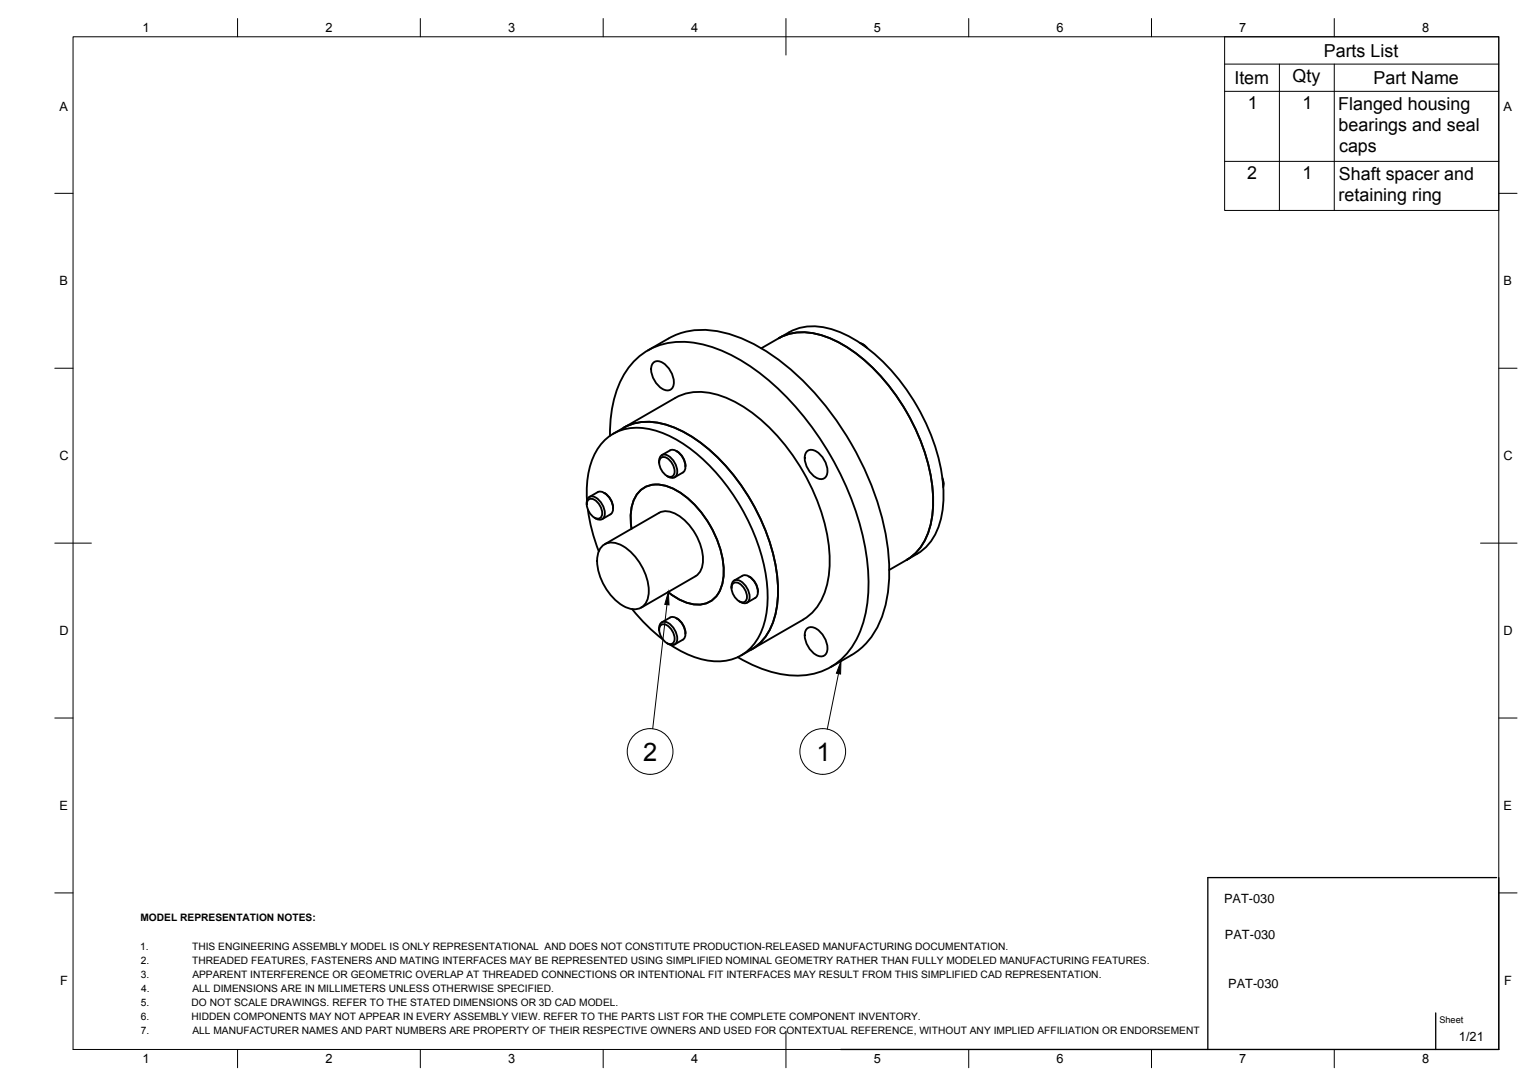
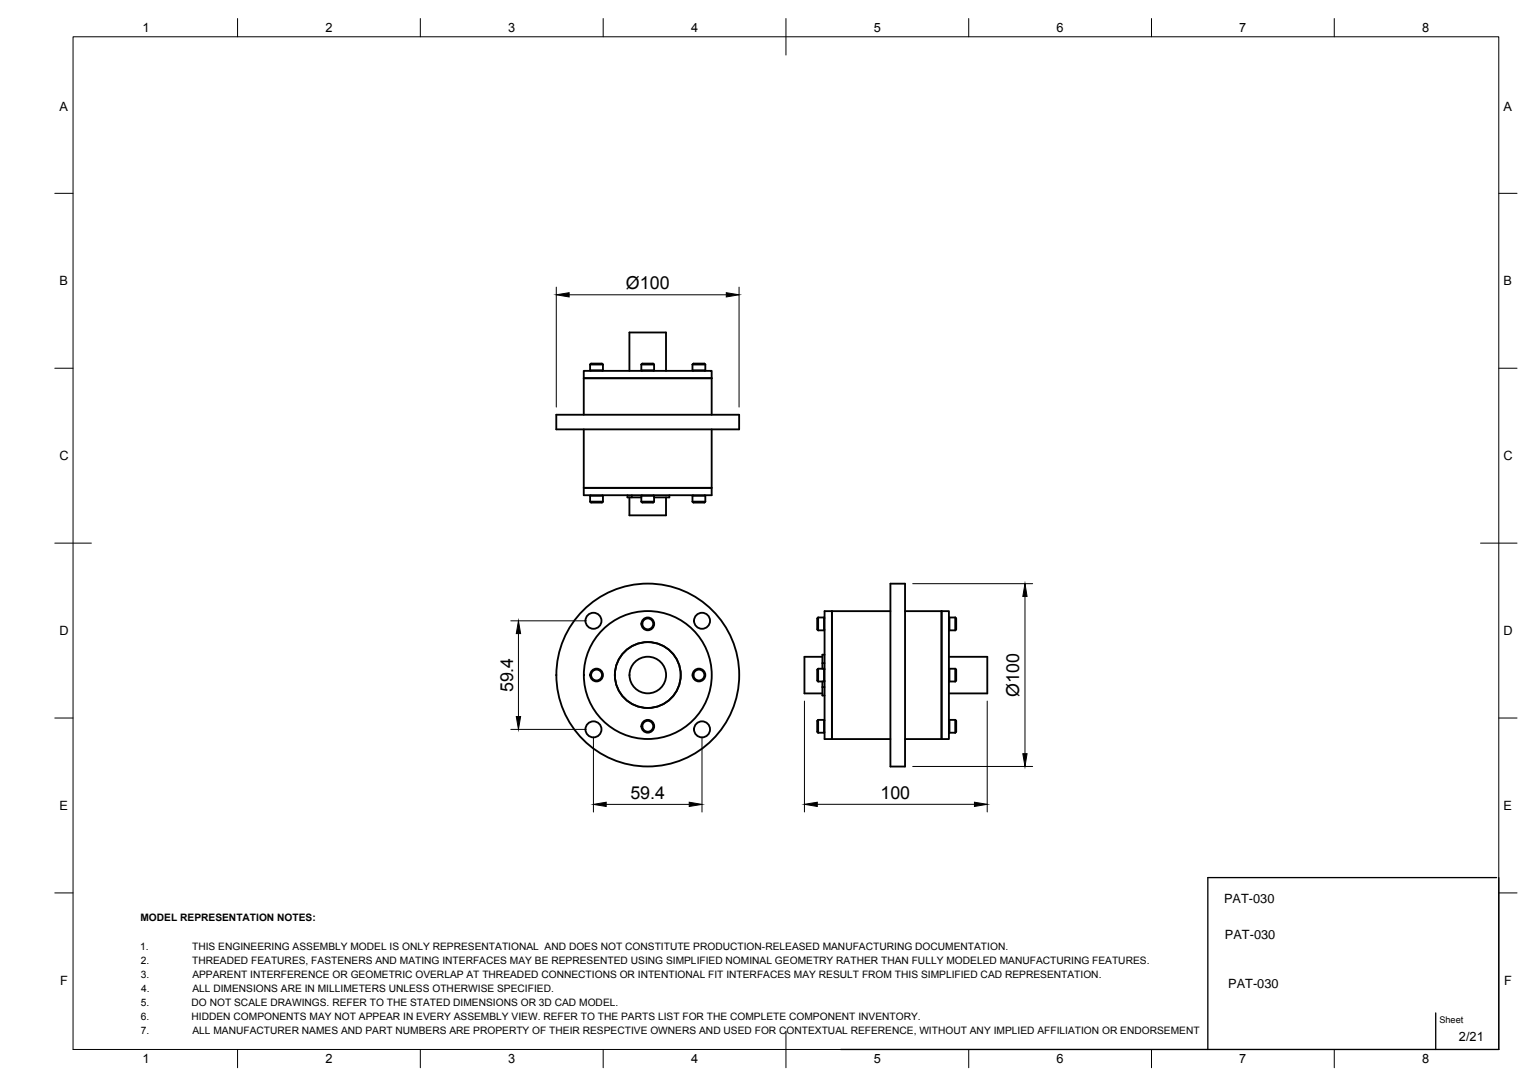
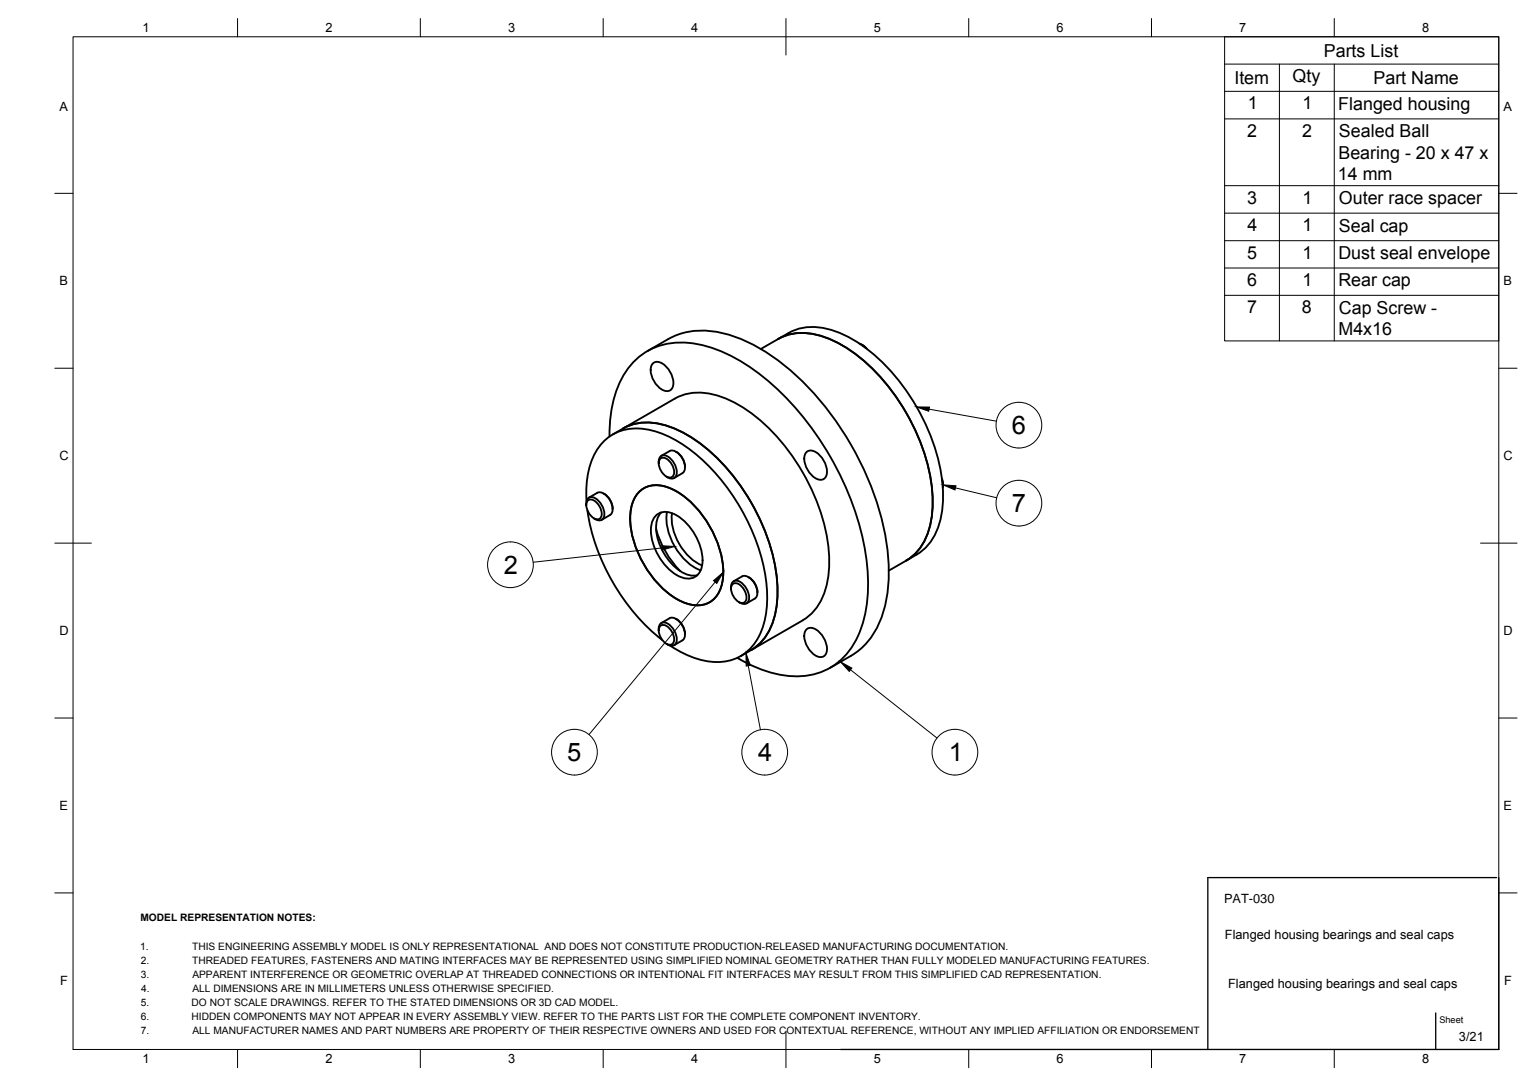
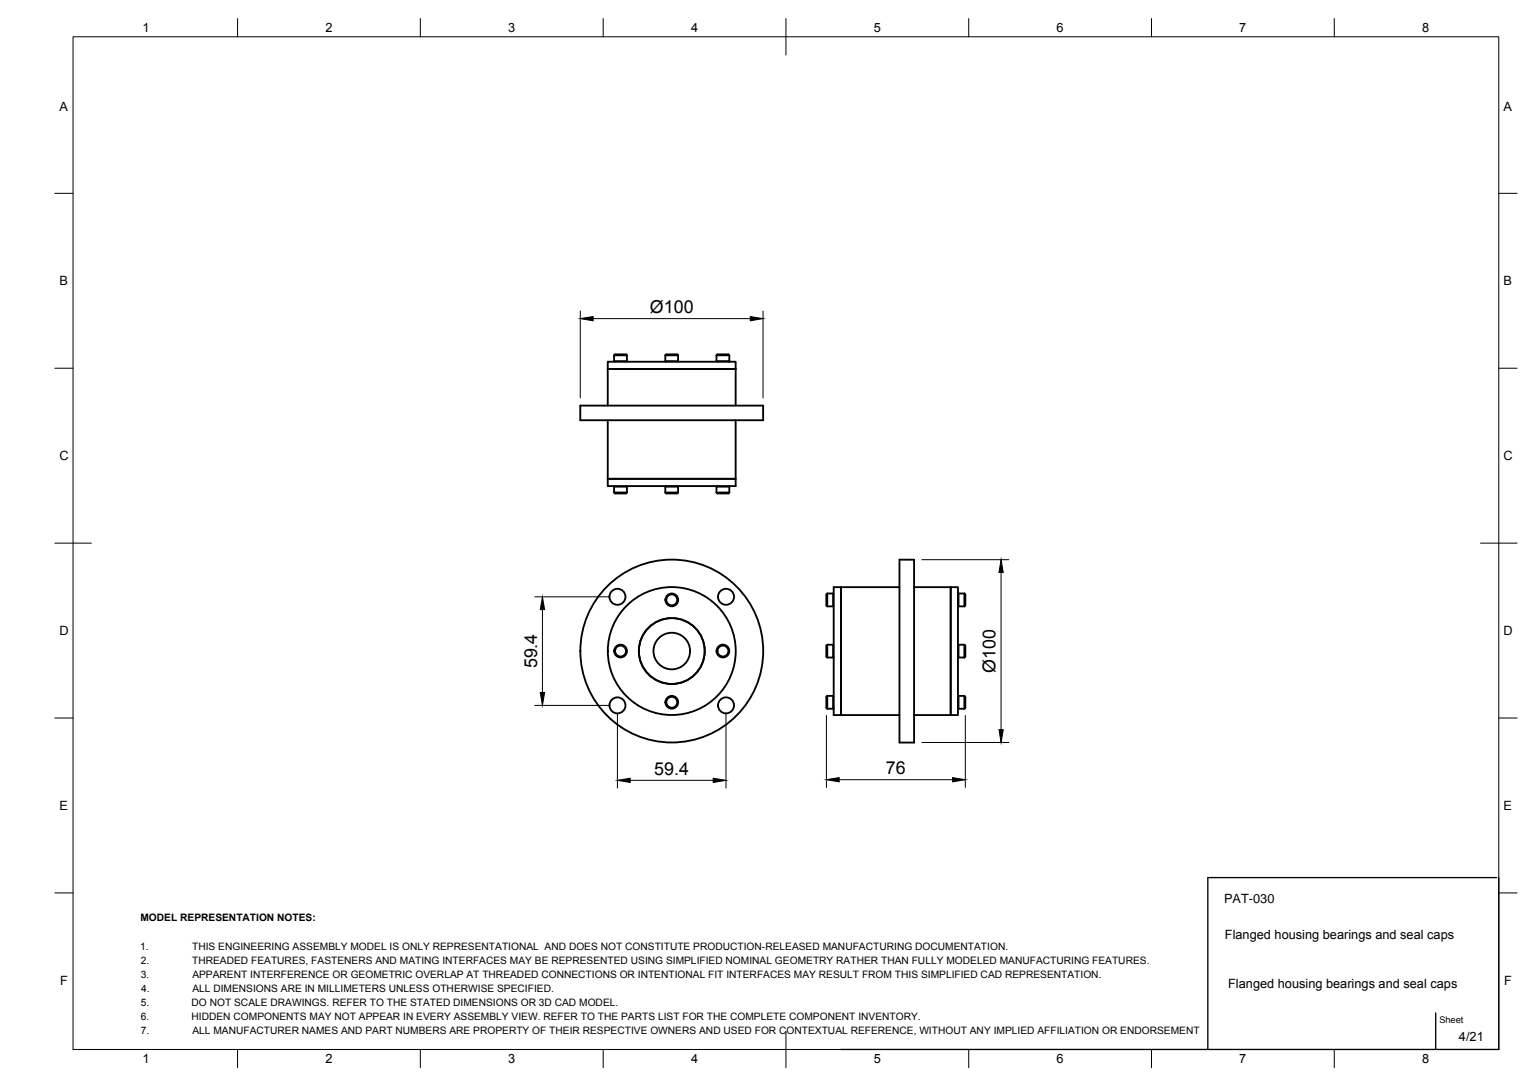
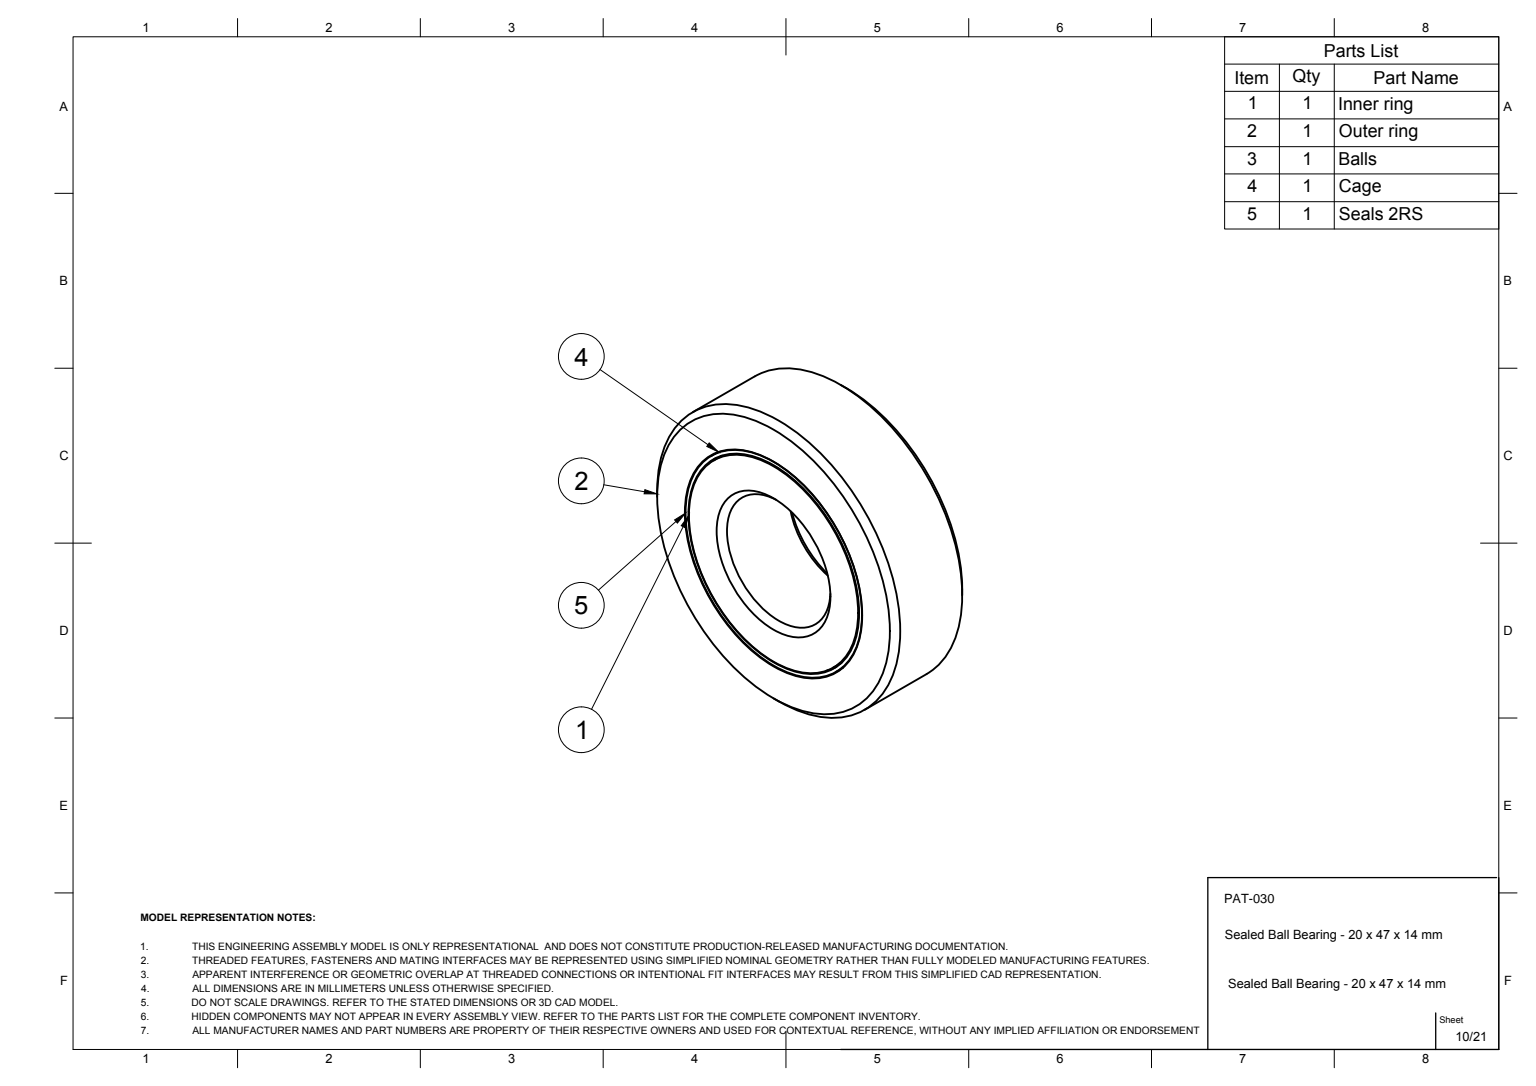
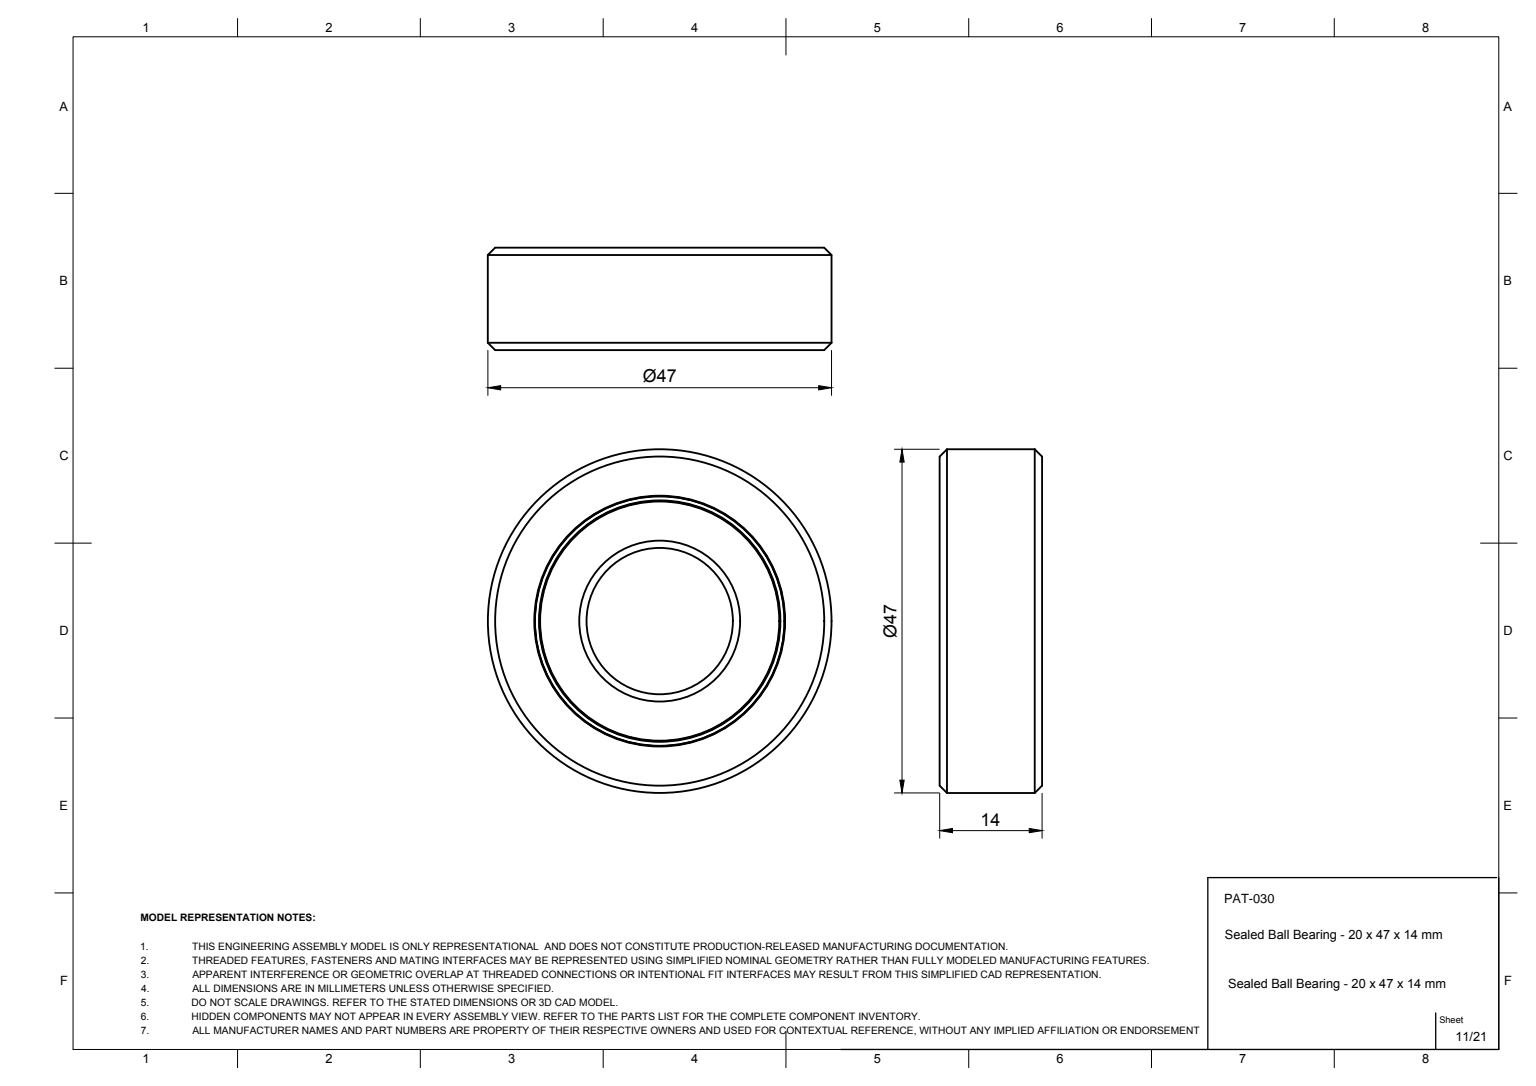
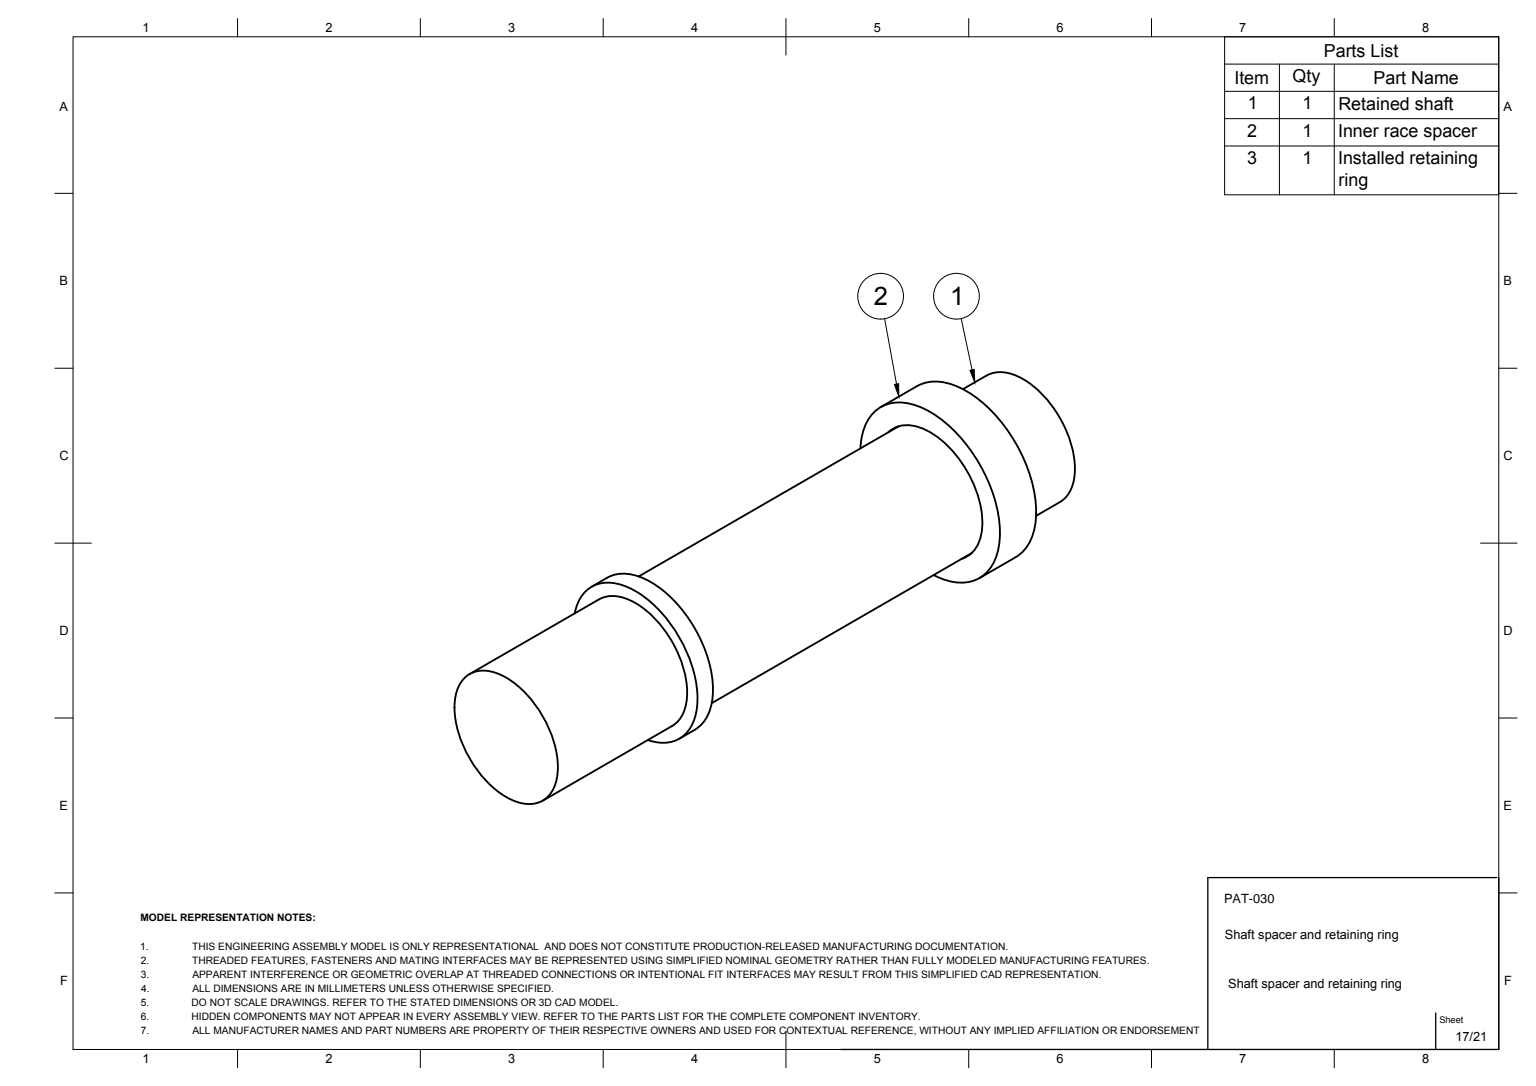
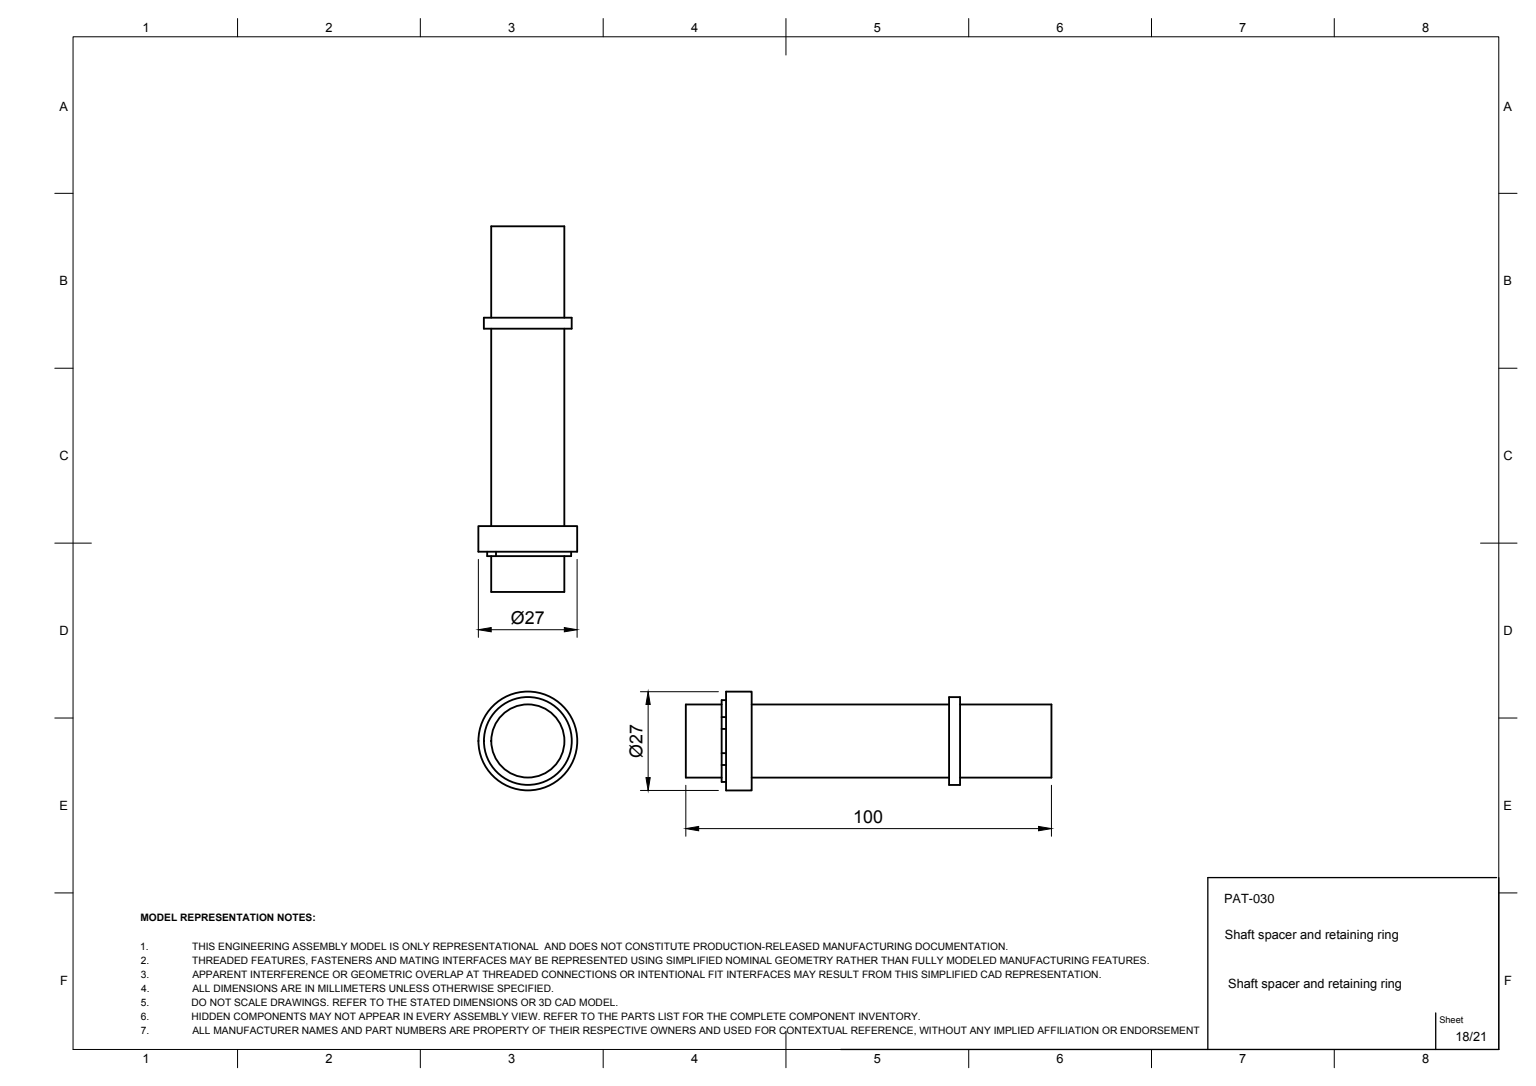
ISO-10303-21;
HEADER;
/* Generated by software containing ST-Developer
 * from STEP Tools, Inc. (www.steptools.com) 
 */

FILE_DESCRIPTION(
/* description */ ('Double-bearing flanged cartridge'),
/* implementation_level */ '2;1');

FILE_NAME(
/* name */ 'PAT-030',
/* time_stamp */ '2026-10-28T03:26:40-07:00',
/* author */ (''),
/* organization */ (''),
/* preprocessor_version */ 'ST-DEVELOPER v20.2',
/* originating_system */ 'Autodesk Translation Framework v15.17.0.0',
/* authorisation */ '');

FILE_SCHEMA (('AUTOMOTIVE_DESIGN { 1 0 10303 214 3 1 1 }'));
ENDSEC;

DATA;
#10=MECHANICAL_DESIGN_GEOMETRIC_PRESENTATION_REPRESENTATION('',(#190,#191,
#192,#193,#194,#195,#196,#197,#198,#199,#200,#201,#202,#203,#204,#205,#206,
#207,#208,#209,#210,#211),#5535);
#11=(
BOUNDED_SURFACE()
B_SPLINE_SURFACE(5,1,((#4887,#4888),(#4889,#4890),(#4891,#4892),(#4893,
#4894),(#4895,#4896),(#4897,#4898),(#4899,#4900),(#4901,#4902),(#4903,#4904),
(#4905,#4906),(#4907,#4908),(#4909,#4910),(#4911,#4912),(#4913,#4914),(#4915,
#4916),(#4917,#4918),(#4919,#4920),(#4921,#4922),(#4923,#4924),(#4925,#4926),
(#4927,#4928),(#4929,#4930),(#4931,#4932),(#4933,#4934),(#4935,#4936),(#4937,
#4938),(#4939,#4940),(#4941,#4942),(#4943,#4944),(#4945,#4946),(#4947,#4948),
(#4949,#4950),(#4951,#4952),(#4953,#4954),(#4955,#4956),(#4957,#4958),(#4959,
#4960),(#4961,#4962),(#4963,#4964),(#4965,#4966),(#4967,#4968),(#4969,#4970),
(#4971,#4972),(#4973,#4974),(#4975,#4976),(#4977,#4978),(#4979,#4980),(#4981,
#4982),(#4983,#4984),(#4985,#4986),(#4987,#4988),(#4989,#4990),(#4991,#4992),
(#4993,#4994),(#4995,#4996),(#4997,#4998),(#4999,#5000),(#5001,#5002),(#5003,
#5004),(#5005,#5006),(#5007,#5008),(#5009,#5010),(#5011,#5012),(#5013,#5014),
(#5015,#5016),(#5017,#5018),(#5019,#5020),(#5021,#5022),(#5023,#5024),(#5025,
#5026),(#5027,#5028),(#5029,#5030),(#5031,#5032),(#5033,#5034),(#5035,#5036),
(#5037,#5038),(#5039,#5040),(#5041,#5042),(#5043,#5044),(#5045,#5046),(#5047,
#5048),(#5049,#5050),(#5051,#5052),(#5053,#5054),(#5055,#5056),(#5057,#5058),
(#5059,#5060),(#5061,#5062),(#5063,#5064),(#5065,#5066),(#5067,#5068),(#5069,
#5070),(#5071,#5072),(#5073,#5074),(#5075,#5076),(#5077,#5078),(#5079,#5080),
(#5081,#5082),(#5083,#5084),(#5085,#5086),(#5087,#5088),(#5089,#5090),(#5091,
#5092),(#5093,#5094),(#5095,#5096),(#5097,#5098),(#5099,#5100),(#5101,#5102),
(#5103,#5104),(#5105,#5106),(#5107,#5108),(#5109,#5110),(#5111,#5112),(#5113,
#5114),(#5115,#5116),(#5117,#5118),(#5119,#5120),(#5121,#5122),(#5123,#5124),
(#5125,#5126),(#5127,#5128),(#5129,#5130),(#5131,#5132),(#5133,#5134),(#5135,
#5136),(#5137,#5138),(#5139,#5140),(#5141,#5142),(#5143,#5144),(#5145,#5146),
(#5147,#5148),(#5149,#5150),(#5151,#5152),(#5153,#5154),(#5155,#5156),(#5157,
#5158),(#5159,#5160),(#5161,#5162),(#5163,#5164),(#5165,#5166),(#5167,#5168),
(#5169,#5170),(#5171,#5172),(#5173,#5174),(#5175,#5176),(#5177,#5178),(#5179,
#5180),(#5181,#5182),(#5183,#5184),(#5185,#5186),(#5187,#5188),(#5189,#5190),
(#5191,#5192),(#5193,#5194),(#5195,#5196),(#5197,#5198),(#5199,#5200),(#5201,
#5202),(#5203,#5204),(#5205,#5206),(#5207,#5208),(#5209,#5210),(#5211,#5212),
(#5213,#5214),(#5215,#5216),(#5217,#5218),(#5219,#5220),(#5221,#5222),(#5223,
#5224),(#5225,#5226),(#5227,#5228),(#5229,#5230),(#5231,#5232),(#5233,#5234),
(#5235,#5236),(#5237,#5238),(#5239,#5240),(#5241,#5242),(#5243,#5244),(#5245,
#5246),(#5247,#5248),(#5249,#5250),(#5251,#5252),(#5253,#5254),(#5255,#5256),
(#5257,#5258),(#5259,#5260),(#5261,#5262),(#5263,#5264),(#5265,#5266),(#5267,
#5268),(#5269,#5270),(#5271,#5272),(#5273,#5274),(#5275,#5276),(#5277,#5278),
(#5279,#5280),(#5281,#5282),(#5283,#5284),(#5285,#5286),(#5287,#5288),(#5289,
#5290),(#5291,#5292),(#5293,#5294),(#5295,#5296)),.UNSPECIFIED.,.F.,.F.,
 .F.)
B_SPLINE_SURFACE_WITH_KNOTS((6,1,1,1,1,1,1,1,1,1,1,1,1,1,1,1,1,1,1,1,1,
1,1,1,1,1,1,1,1,1,1,1,1,1,1,1,1,1,1,1,1,1,1,1,1,1,1,1,1,1,1,1,1,1,1,1,1,
1,1,1,1,1,1,1,1,1,1,1,1,1,1,1,1,1,1,1,1,1,1,1,1,1,1,1,1,1,1,1,1,1,1,1,1,
1,1,1,1,1,1,1,1,1,1,1,1,1,1,1,1,1,1,1,1,1,1,1,1,1,1,1,1,1,1,1,1,1,1,1,1,
1,1,1,1,1,1,1,1,1,1,1,1,1,1,1,1,1,1,1,1,1,1,1,1,1,1,1,1,1,1,1,1,1,1,1,1,
1,1,1,1,1,1,1,1,1,1,1,1,1,1,1,1,1,1,1,1,1,1,1,1,1,1,1,1,1,1,1,1,1,1,1,6),
(2,2),(0.,0.005,0.01,0.015,0.02,0.025,0.03,0.035,0.04,0.045,0.05,0.055,
0.06,0.065,0.07,0.075,0.08,0.085,0.09,0.095,0.1,0.105,0.11,0.115,0.12,0.125,
0.13,0.135,0.14,0.145,0.15,0.155,0.16,0.165,0.17,0.175,0.18,0.185,0.19,
0.195,0.2,0.205,0.21,0.215,0.22,0.225,0.23,0.235,0.24,0.245,0.25,0.255,
0.26,0.265,0.27,0.275,0.28,0.285,0.29,0.295,0.3,0.305,0.31,0.315,0.32,0.325,
0.33,0.335,0.34,0.345,0.35,0.355,0.36,0.365,0.37,0.375,0.38,0.385,0.39,
0.395,0.4,0.405,0.41,0.415,0.42,0.425,0.43,0.435,0.44,0.445,0.45,0.455,
0.46,0.465,0.47,0.475,0.48,0.485,0.49,0.495,0.5,0.505,0.51,0.515,0.52,0.525,
0.53,0.535,0.54,0.545,0.55,0.555,0.56,0.565,0.57,0.575,0.58,0.585,0.59,
0.595,0.6,0.605,0.61,0.615,0.62,0.625,0.63,0.635,0.64,0.645,0.65,0.655,
0.66,0.665,0.67,0.675,0.68,0.685,0.690000000000001,0.695000000000001,0.700000000000001,
0.705000000000001,0.710000000000001,0.715000000000001,0.720000000000001,
0.725000000000001,0.730000000000001,0.735000000000001,0.740000000000001,
0.745000000000001,0.750000000000001,0.755000000000001,0.760000000000001,
0.765000000000001,0.770000000000001,0.775000000000001,0.780000000000001,
0.785000000000001,0.790000000000001,0.795000000000001,0.800000000000001,
0.805000000000001,0.810000000000001,0.815000000000001,0.820000000000001,
0.825000000000001,0.830000000000001,0.835000000000001,0.840000000000001,
0.845000000000001,0.850000000000001,0.855000000000001,0.860000000000001,
0.865000000000001,0.870000000000001,0.875000000000001,0.880000000000001,
0.885000000000001,0.890000000000001,0.895000000000001,0.900000000000001,
0.905000000000001,0.910000000000001,0.915000000000001,0.920000000000001,
0.925000000000001,0.930000000000001,0.935000000000001,0.940000000000001,
0.945000000000001,0.950000000000001,0.955000000000001,0.960000000000001,
0.965000000000001,0.970000000000001,0.975000000000001,0.980000000000001,
0.985000000000001,0.990000000000001,0.995000000000001,1.),(0.,0.12),
 .UNSPECIFIED.)
GEOMETRIC_REPRESENTATION_ITEM()
RATIONAL_B_SPLINE_SURFACE(((1.,1.),(1.,1.),(1.,1.),(1.,1.),(1.,1.),(1.,
1.),(1.,1.),(1.,1.),(1.,1.),(1.,1.),(1.,1.),(1.,1.),(1.,1.),(1.,1.),(1.,
1.),(1.,1.),(1.,1.),(1.,1.),(1.,1.),(1.,1.),(1.,1.),(1.,1.),(1.,1.),(1.,
1.),(1.,1.),(1.,1.),(1.,1.),(1.,1.),(1.,1.),(1.,1.),(1.,1.),(1.,1.),(1.,
1.),(1.,1.),(1.,1.),(1.,1.),(1.,1.),(1.,1.),(1.,1.),(1.,1.),(1.,1.),(1.,
1.),(1.,1.),(1.,1.),(1.,1.),(1.,1.),(1.,1.),(1.,1.),(1.,1.),(1.,1.),(1.,
1.),(1.,1.),(1.,1.),(1.,1.),(1.,1.),(1.,1.),(1.,1.),(1.,1.),(1.,1.),(1.,
1.),(1.,1.),(1.,1.),(1.,1.),(1.,1.),(1.,1.),(1.,1.),(1.,1.),(1.,1.),(1.,
1.),(1.,1.),(1.,1.),(1.,1.),(1.,1.),(1.,1.),(1.,1.),(1.,1.),(1.,1.),(1.,
1.),(1.,1.),(1.,1.),(1.,1.),(1.,1.),(1.,1.),(1.,1.),(1.,1.),(1.,1.),(1.,
1.),(1.,1.),(1.,1.),(1.,1.),(1.,1.),(1.,1.),(1.,1.),(1.,1.),(1.,1.),(1.,
1.),(1.,1.),(1.,1.),(1.,1.),(1.,1.),(1.,1.),(1.,1.),(1.,1.),(1.,1.),(1.,
1.),(1.,1.),(1.,1.),(1.,1.),(1.,1.),(1.,1.),(1.,1.),(1.,1.),(1.,1.),(1.,
1.),(1.,1.),(1.,1.),(1.,1.),(1.,1.),(1.,1.),(1.,1.),(1.,1.),(1.,1.),(1.,
1.),(1.,1.),(1.,1.),(1.,1.),(1.,1.),(1.,1.),(1.,1.),(1.,1.),(1.,1.),(1.,
1.),(1.,1.),(1.,1.),(1.,1.),(1.,1.),(1.,1.),(1.,1.),(1.,1.),(1.,1.),(1.,
1.),(1.,1.),(1.,1.),(1.,1.),(1.,1.),(1.,1.),(1.,1.),(1.,1.),(1.,1.),(1.,
1.),(1.,1.),(1.,1.),(1.,1.),(1.,1.),(1.,1.),(1.,1.),(1.,1.),(1.,1.),(1.,
1.),(1.,1.),(1.,1.),(1.,1.),(1.,1.),(1.,1.),(1.,1.),(1.,1.),(1.,1.),(1.,
1.),(1.,1.),(1.,1.),(1.,1.),(1.,1.),(1.,1.),(1.,1.),(1.,1.),(1.,1.),(1.,
1.),(1.,1.),(1.,1.),(1.,1.),(1.,1.),(1.,1.),(1.,1.),(1.,1.),(1.,1.),(1.,
1.),(1.,1.),(1.,1.),(1.,1.),(1.,1.),(1.,1.),(1.,1.),(1.,1.),(1.,1.),(1.,
1.),(1.,1.),(1.,1.),(1.,1.),(1.,1.),(1.,1.),(1.,1.),(1.,1.),(1.,1.),(1.,
1.),(1.,1.)))
REPRESENTATION_ITEM('')
SURFACE()
);
#12=(
BOUNDED_CURVE()
B_SPLINE_CURVE(5,(#4671,#4672,#4673,#4674,#4675,#4676,#4677,#4678,#4679,
#4680,#4681,#4682,#4683,#4684,#4685,#4686,#4687,#4688,#4689,#4690,#4691,
#4692,#4693,#4694,#4695,#4696,#4697,#4698,#4699,#4700,#4701,#4702,#4703,
#4704,#4705,#4706,#4707,#4708,#4709,#4710,#4711,#4712,#4713,#4714,#4715,
#4716,#4717,#4718,#4719,#4720,#4721,#4722,#4723,#4724,#4725,#4726,#4727,
#4728,#4729,#4730,#4731,#4732,#4733,#4734,#4735,#4736,#4737,#4738,#4739,
#4740,#4741,#4742,#4743,#4744,#4745,#4746,#4747,#4748,#4749,#4750,#4751,
#4752,#4753,#4754,#4755,#4756,#4757,#4758,#4759,#4760,#4761,#4762,#4763,
#4764,#4765,#4766,#4767,#4768,#4769,#4770,#4771,#4772,#4773,#4774,#4775,
#4776,#4777,#4778,#4779,#4780,#4781,#4782,#4783,#4784,#4785,#4786,#4787,
#4788,#4789,#4790,#4791,#4792,#4793,#4794,#4795,#4796,#4797,#4798,#4799,
#4800,#4801,#4802,#4803,#4804,#4805,#4806,#4807,#4808,#4809,#4810,#4811,
#4812,#4813,#4814,#4815,#4816,#4817,#4818,#4819,#4820,#4821,#4822,#4823,
#4824,#4825,#4826,#4827,#4828,#4829,#4830,#4831,#4832,#4833,#4834,#4835,
#4836,#4837,#4838,#4839,#4840,#4841,#4842,#4843,#4844,#4845,#4846,#4847,
#4848,#4849,#4850,#4851,#4852,#4853,#4854,#4855,#4856,#4857,#4858,#4859,
#4860,#4861,#4862,#4863,#4864,#4865),.UNSPECIFIED.,.F.,.F.)
B_SPLINE_CURVE_WITH_KNOTS((6,1,1,1,1,1,1,1,1,1,1,1,1,1,1,1,1,1,1,1,1,1,
1,1,1,1,1,1,1,1,1,1,1,1,1,1,1,1,1,1,1,1,1,1,1,1,1,1,1,1,1,1,1,1,1,1,1,1,
1,1,1,1,1,1,1,1,1,1,1,1,1,1,1,1,1,1,1,1,1,1,1,1,1,1,1,1,1,1,1,1,1,1,1,1,
1,1,1,1,1,1,1,1,1,1,1,1,1,1,1,1,1,1,1,1,1,1,1,1,1,1,1,1,1,1,1,1,1,1,1,1,
1,1,1,1,1,1,1,1,1,1,1,1,1,1,1,1,1,1,1,1,1,1,1,1,1,1,1,1,1,1,1,1,1,1,1,1,
1,1,1,1,1,1,1,1,1,1,1,1,1,1,1,1,1,1,1,1,1,1,1,1,6),(0.02759962388435,0.03,
0.035,0.04,0.045,0.05,0.055,0.06,0.065,0.07,0.075,0.08,0.085,0.09,0.095,
0.1,0.105,0.11,0.115,0.12,0.125,0.13,0.135,0.14,0.145,0.15,0.155,0.16,0.165,
0.17,0.175,0.18,0.185,0.19,0.195,0.2,0.205,0.21,0.215,0.22,0.225,0.23,0.235,
0.24,0.245,0.25,0.255,0.26,0.265,0.27,0.275,0.28,0.285,0.29,0.295,0.3,0.305,
0.31,0.315,0.32,0.325,0.33,0.335,0.34,0.345,0.35,0.355,0.36,0.365,0.37,
0.375,0.38,0.385,0.39,0.395,0.4,0.405,0.41,0.415,0.42,0.425,0.43,0.435,
0.44,0.445,0.45,0.455,0.46,0.465,0.47,0.475,0.48,0.485,0.49,0.495,0.5,0.505,
0.51,0.515,0.52,0.525,0.53,0.535,0.54,0.545,0.55,0.555,0.56,0.565,0.57,
0.575,0.58,0.585,0.59,0.595,0.6,0.605,0.61,0.615,0.62,0.625,0.63,0.635,
0.64,0.645,0.65,0.655,0.66,0.665,0.67,0.675,0.68,0.685,0.690000000000001,
0.695000000000001,0.700000000000001,0.705000000000001,0.710000000000001,
0.715000000000001,0.720000000000001,0.725000000000001,0.730000000000001,
0.735000000000001,0.740000000000001,0.745000000000001,0.750000000000001,
0.755000000000001,0.760000000000001,0.765000000000001,0.770000000000001,
0.775000000000001,0.780000000000001,0.785000000000001,0.790000000000001,
0.795000000000001,0.800000000000001,0.805000000000001,0.810000000000001,
0.815000000000001,0.820000000000001,0.825000000000001,0.830000000000001,
0.835000000000001,0.840000000000001,0.845000000000001,0.850000000000001,
0.855000000000001,0.860000000000001,0.865000000000001,0.870000000000001,
0.875000000000001,0.880000000000001,0.885000000000001,0.890000000000001,
0.895000000000001,0.900000000000001,0.905000000000001,0.910000000000001,
0.915000000000001,0.920000000000001,0.925000000000001,0.930000000000001,
0.935000000000001,0.940000000000001,0.945000000000001,0.950000000000001,
0.955000000000001,0.960000000000001,0.965000000000001,0.970000000000001,
0.972400376115677),.UNSPECIFIED.)
CURVE()
GEOMETRIC_REPRESENTATION_ITEM()
RATIONAL_B_SPLINE_CURVE((1.,1.,1.,1.,1.,1.,1.,1.,1.,1.,1.,1.,1.,1.,1.,1.,
1.,1.,1.,1.,1.,1.,1.,1.,1.,1.,1.,1.,1.,1.,1.,1.,1.,1.,1.,1.,1.,1.,1.,1.,
1.,1.,1.,1.,1.,1.,1.,1.,1.,1.,1.,1.,1.,1.,1.,1.,1.,1.,1.,1.,1.,1.,1.,1.,
1.,1.,1.,1.,1.,1.,1.,1.,1.,1.,1.,1.,1.,1.,1.,1.,1.,1.,1.,1.,1.,1.,1.,1.,
1.,1.,1.,1.,1.,1.,1.,1.,1.,1.,1.,1.,1.,1.,1.,1.,1.,1.,1.,1.,1.,1.,1.,1.,
1.,1.,1.,1.,1.,1.,1.,1.,1.,1.,1.,1.,1.,1.,1.,1.,1.,1.,1.,1.,1.,1.,1.,1.,
1.,1.,1.,1.,1.,1.,1.,1.,1.,1.,1.,1.,1.,1.,1.,1.,1.,1.,1.,1.,1.,1.,1.,1.,
1.,1.,1.,1.,1.,1.,1.,1.,1.,1.,1.,1.,1.,1.,1.,1.,1.,1.,1.,1.,1.,1.,1.,1.,
1.,1.,1.,1.,1.,1.,1.,1.,1.,1.,1.))
REPRESENTATION_ITEM('')
);
#13=(
BOUNDED_CURVE()
B_SPLINE_CURVE(5,(#5297,#5298,#5299,#5300,#5301,#5302,#5303,#5304,#5305,
#5306,#5307,#5308,#5309,#5310,#5311,#5312,#5313,#5314,#5315,#5316,#5317,
#5318,#5319,#5320,#5321,#5322,#5323,#5324,#5325,#5326,#5327,#5328,#5329,
#5330,#5331,#5332,#5333,#5334,#5335,#5336,#5337,#5338,#5339,#5340,#5341,
#5342,#5343,#5344,#5345,#5346,#5347,#5348,#5349,#5350,#5351,#5352,#5353,
#5354,#5355,#5356,#5357,#5358,#5359,#5360,#5361,#5362,#5363,#5364,#5365,
#5366,#5367,#5368,#5369,#5370,#5371,#5372,#5373,#5374,#5375,#5376,#5377,
#5378,#5379,#5380,#5381,#5382,#5383,#5384,#5385,#5386,#5387,#5388,#5389,
#5390,#5391,#5392,#5393,#5394,#5395,#5396,#5397,#5398,#5399,#5400,#5401,
#5402,#5403,#5404,#5405,#5406,#5407,#5408,#5409,#5410,#5411,#5412,#5413,
#5414,#5415,#5416,#5417,#5418,#5419,#5420,#5421,#5422,#5423,#5424,#5425,
#5426,#5427,#5428,#5429,#5430,#5431,#5432,#5433,#5434,#5435,#5436,#5437,
#5438,#5439,#5440,#5441,#5442,#5443,#5444,#5445,#5446,#5447,#5448,#5449,
#5450,#5451,#5452,#5453,#5454,#5455,#5456,#5457,#5458,#5459,#5460,#5461,
#5462,#5463,#5464,#5465,#5466,#5467,#5468,#5469,#5470,#5471,#5472,#5473,
#5474,#5475,#5476,#5477,#5478,#5479,#5480,#5481,#5482,#5483,#5484,#5485,
#5486,#5487,#5488,#5489,#5490,#5491),.UNSPECIFIED.,.F.,.F.)
B_SPLINE_CURVE_WITH_KNOTS((6,1,1,1,1,1,1,1,1,1,1,1,1,1,1,1,1,1,1,1,1,1,
1,1,1,1,1,1,1,1,1,1,1,1,1,1,1,1,1,1,1,1,1,1,1,1,1,1,1,1,1,1,1,1,1,1,1,1,
1,1,1,1,1,1,1,1,1,1,1,1,1,1,1,1,1,1,1,1,1,1,1,1,1,1,1,1,1,1,1,1,1,1,1,1,
1,1,1,1,1,1,1,1,1,1,1,1,1,1,1,1,1,1,1,1,1,1,1,1,1,1,1,1,1,1,1,1,1,1,1,1,
1,1,1,1,1,1,1,1,1,1,1,1,1,1,1,1,1,1,1,1,1,1,1,1,1,1,1,1,1,1,1,1,1,1,1,1,
1,1,1,1,1,1,1,1,1,1,1,1,1,1,1,1,1,1,1,1,1,1,1,1,6),(0.02759962388435,0.03,
0.035,0.04,0.045,0.05,0.055,0.06,0.065,0.07,0.075,0.08,0.085,0.09,0.095,
0.1,0.105,0.11,0.115,0.12,0.125,0.13,0.135,0.14,0.145,0.15,0.155,0.16,0.165,
0.17,0.175,0.18,0.185,0.19,0.195,0.2,0.205,0.21,0.215,0.22,0.225,0.23,0.235,
0.24,0.245,0.25,0.255,0.26,0.265,0.27,0.275,0.28,0.285,0.29,0.295,0.3,0.305,
0.31,0.315,0.32,0.325,0.33,0.335,0.34,0.345,0.35,0.355,0.36,0.365,0.37,
0.375,0.38,0.385,0.39,0.395,0.4,0.405,0.41,0.415,0.42,0.425,0.43,0.435,
0.44,0.445,0.45,0.455,0.46,0.465,0.47,0.475,0.48,0.485,0.49,0.495,0.5,0.505,
0.51,0.515,0.52,0.525,0.53,0.535,0.54,0.545,0.55,0.555,0.56,0.565,0.57,
0.575,0.58,0.585,0.59,0.595,0.6,0.605,0.61,0.615,0.62,0.625,0.63,0.635,
0.64,0.645,0.65,0.655,0.66,0.665,0.67,0.675,0.68,0.685,0.690000000000001,
0.695000000000001,0.700000000000001,0.705000000000001,0.710000000000001,
0.715000000000001,0.720000000000001,0.725000000000001,0.730000000000001,
0.735000000000001,0.740000000000001,0.745000000000001,0.750000000000001,
0.755000000000001,0.760000000000001,0.765000000000001,0.770000000000001,
0.775000000000001,0.780000000000001,0.785000000000001,0.790000000000001,
0.795000000000001,0.800000000000001,0.805000000000001,0.810000000000001,
0.815000000000001,0.820000000000001,0.825000000000001,0.830000000000001,
0.835000000000001,0.840000000000001,0.845000000000001,0.850000000000001,
0.855000000000001,0.860000000000001,0.865000000000001,0.870000000000001,
0.875000000000001,0.880000000000001,0.885000000000001,0.890000000000001,
0.895000000000001,0.900000000000001,0.905000000000001,0.910000000000001,
0.915000000000001,0.920000000000001,0.925000000000001,0.930000000000001,
0.935000000000001,0.940000000000001,0.945000000000001,0.950000000000001,
0.955000000000001,0.960000000000001,0.965000000000001,0.970000000000001,
0.972400376115677),.UNSPECIFIED.)
CURVE()
GEOMETRIC_REPRESENTATION_ITEM()
RATIONAL_B_SPLINE_CURVE((1.,1.,1.,1.,1.,1.,1.,1.,1.,1.,1.,1.,1.,1.,1.,1.,
1.,1.,1.,1.,1.,1.,1.,1.,1.,1.,1.,1.,1.,1.,1.,1.,1.,1.,1.,1.,1.,1.,1.,1.,
1.,1.,1.,1.,1.,1.,1.,1.,1.,1.,1.,1.,1.,1.,1.,1.,1.,1.,1.,1.,1.,1.,1.,1.,
1.,1.,1.,1.,1.,1.,1.,1.,1.,1.,1.,1.,1.,1.,1.,1.,1.,1.,1.,1.,1.,1.,1.,1.,
1.,1.,1.,1.,1.,1.,1.,1.,1.,1.,1.,1.,1.,1.,1.,1.,1.,1.,1.,1.,1.,1.,1.,1.,
1.,1.,1.,1.,1.,1.,1.,1.,1.,1.,1.,1.,1.,1.,1.,1.,1.,1.,1.,1.,1.,1.,1.,1.,
1.,1.,1.,1.,1.,1.,1.,1.,1.,1.,1.,1.,1.,1.,1.,1.,1.,1.,1.,1.,1.,1.,1.,1.,
1.,1.,1.,1.,1.,1.,1.,1.,1.,1.,1.,1.,1.,1.,1.,1.,1.,1.,1.,1.,1.,1.,1.,1.,
1.,1.,1.,1.,1.,1.,1.,1.,1.,1.,1.))
REPRESENTATION_ITEM('')
);
#14=ORIENTED_CLOSED_SHELL('',*,#2343,.F.);
#15=BREP_WITH_VOIDS('Body1',#2342,(#14));
#16=ITEM_DEFINED_TRANSFORMATION($,$,#2566,#2694);
#17=ITEM_DEFINED_TRANSFORMATION($,$,#2586,#2695);
#18=ITEM_DEFINED_TRANSFORMATION($,$,#2606,#2696);
#19=ITEM_DEFINED_TRANSFORMATION($,$,#2623,#2697);
#20=ITEM_DEFINED_TRANSFORMATION($,$,#2677,#2698);
#21=ITEM_DEFINED_TRANSFORMATION($,$,#2504,#2797);
#22=ITEM_DEFINED_TRANSFORMATION($,$,#2565,#2798);
#23=ITEM_DEFINED_TRANSFORMATION($,$,#2565,#2799);
#24=ITEM_DEFINED_TRANSFORMATION($,$,#2699,#2800);
#25=ITEM_DEFINED_TRANSFORMATION($,$,#2708,#2801);
#26=ITEM_DEFINED_TRANSFORMATION($,$,#2737,#2802);
#27=ITEM_DEFINED_TRANSFORMATION($,$,#2746,#2803);
#28=ITEM_DEFINED_TRANSFORMATION($,$,#2771,#2804);
#29=ITEM_DEFINED_TRANSFORMATION($,$,#2771,#2805);
#30=ITEM_DEFINED_TRANSFORMATION($,$,#2771,#2806);
#31=ITEM_DEFINED_TRANSFORMATION($,$,#2771,#2807);
#32=ITEM_DEFINED_TRANSFORMATION($,$,#2771,#2808);
#33=ITEM_DEFINED_TRANSFORMATION($,$,#2771,#2809);
#34=ITEM_DEFINED_TRANSFORMATION($,$,#2771,#2810);
#35=ITEM_DEFINED_TRANSFORMATION($,$,#2771,#2811);
#36=ITEM_DEFINED_TRANSFORMATION($,$,#2813,#2862);
#37=ITEM_DEFINED_TRANSFORMATION($,$,#2835,#2863);
#38=ITEM_DEFINED_TRANSFORMATION($,$,#2844,#2864);
#39=ITEM_DEFINED_TRANSFORMATION($,$,#2503,#2865);
#40=ITEM_DEFINED_TRANSFORMATION($,$,#2812,#2866);
#41=(
REPRESENTATION_RELATIONSHIP($,$,#5605,#5604)
REPRESENTATION_RELATIONSHIP_WITH_TRANSFORMATION(#16)
SHAPE_REPRESENTATION_RELATIONSHIP()
);
#42=(
REPRESENTATION_RELATIONSHIP($,$,#5606,#5604)
REPRESENTATION_RELATIONSHIP_WITH_TRANSFORMATION(#17)
SHAPE_REPRESENTATION_RELATIONSHIP()
);
#43=(
REPRESENTATION_RELATIONSHIP($,$,#5607,#5604)
REPRESENTATION_RELATIONSHIP_WITH_TRANSFORMATION(#18)
SHAPE_REPRESENTATION_RELATIONSHIP()
);
#44=(
REPRESENTATION_RELATIONSHIP($,$,#5608,#5604)
REPRESENTATION_RELATIONSHIP_WITH_TRANSFORMATION(#19)
SHAPE_REPRESENTATION_RELATIONSHIP()
);
#45=(
REPRESENTATION_RELATIONSHIP($,$,#5609,#5604)
REPRESENTATION_RELATIONSHIP_WITH_TRANSFORMATION(#20)
SHAPE_REPRESENTATION_RELATIONSHIP()
);
#46=(
REPRESENTATION_RELATIONSHIP($,$,#5603,#5602)
REPRESENTATION_RELATIONSHIP_WITH_TRANSFORMATION(#21)
SHAPE_REPRESENTATION_RELATIONSHIP()
);
#47=(
REPRESENTATION_RELATIONSHIP($,$,#5604,#5602)
REPRESENTATION_RELATIONSHIP_WITH_TRANSFORMATION(#22)
SHAPE_REPRESENTATION_RELATIONSHIP()
);
#48=(
REPRESENTATION_RELATIONSHIP($,$,#5604,#5602)
REPRESENTATION_RELATIONSHIP_WITH_TRANSFORMATION(#23)
SHAPE_REPRESENTATION_RELATIONSHIP()
);
#49=(
REPRESENTATION_RELATIONSHIP($,$,#5610,#5602)
REPRESENTATION_RELATIONSHIP_WITH_TRANSFORMATION(#24)
SHAPE_REPRESENTATION_RELATIONSHIP()
);
#50=(
REPRESENTATION_RELATIONSHIP($,$,#5611,#5602)
REPRESENTATION_RELATIONSHIP_WITH_TRANSFORMATION(#25)
SHAPE_REPRESENTATION_RELATIONSHIP()
);
#51=(
REPRESENTATION_RELATIONSHIP($,$,#5612,#5602)
REPRESENTATION_RELATIONSHIP_WITH_TRANSFORMATION(#26)
SHAPE_REPRESENTATION_RELATIONSHIP()
);
#52=(
REPRESENTATION_RELATIONSHIP($,$,#5613,#5602)
REPRESENTATION_RELATIONSHIP_WITH_TRANSFORMATION(#27)
SHAPE_REPRESENTATION_RELATIONSHIP()
);
#53=(
REPRESENTATION_RELATIONSHIP($,$,#5614,#5602)
REPRESENTATION_RELATIONSHIP_WITH_TRANSFORMATION(#28)
SHAPE_REPRESENTATION_RELATIONSHIP()
);
#54=(
REPRESENTATION_RELATIONSHIP($,$,#5614,#5602)
REPRESENTATION_RELATIONSHIP_WITH_TRANSFORMATION(#29)
SHAPE_REPRESENTATION_RELATIONSHIP()
);
#55=(
REPRESENTATION_RELATIONSHIP($,$,#5614,#5602)
REPRESENTATION_RELATIONSHIP_WITH_TRANSFORMATION(#30)
SHAPE_REPRESENTATION_RELATIONSHIP()
);
#56=(
REPRESENTATION_RELATIONSHIP($,$,#5614,#5602)
REPRESENTATION_RELATIONSHIP_WITH_TRANSFORMATION(#31)
SHAPE_REPRESENTATION_RELATIONSHIP()
);
#57=(
REPRESENTATION_RELATIONSHIP($,$,#5614,#5602)
REPRESENTATION_RELATIONSHIP_WITH_TRANSFORMATION(#32)
SHAPE_REPRESENTATION_RELATIONSHIP()
);
#58=(
REPRESENTATION_RELATIONSHIP($,$,#5614,#5602)
REPRESENTATION_RELATIONSHIP_WITH_TRANSFORMATION(#33)
SHAPE_REPRESENTATION_RELATIONSHIP()
);
#59=(
REPRESENTATION_RELATIONSHIP($,$,#5614,#5602)
REPRESENTATION_RELATIONSHIP_WITH_TRANSFORMATION(#34)
SHAPE_REPRESENTATION_RELATIONSHIP()
);
#60=(
REPRESENTATION_RELATIONSHIP($,$,#5614,#5602)
REPRESENTATION_RELATIONSHIP_WITH_TRANSFORMATION(#35)
SHAPE_REPRESENTATION_RELATIONSHIP()
);
#61=(
REPRESENTATION_RELATIONSHIP($,$,#5616,#5615)
REPRESENTATION_RELATIONSHIP_WITH_TRANSFORMATION(#36)
SHAPE_REPRESENTATION_RELATIONSHIP()
);
#62=(
REPRESENTATION_RELATIONSHIP($,$,#5617,#5615)
REPRESENTATION_RELATIONSHIP_WITH_TRANSFORMATION(#37)
SHAPE_REPRESENTATION_RELATIONSHIP()
);
#63=(
REPRESENTATION_RELATIONSHIP($,$,#5618,#5615)
REPRESENTATION_RELATIONSHIP_WITH_TRANSFORMATION(#38)
SHAPE_REPRESENTATION_RELATIONSHIP()
);
#64=(
REPRESENTATION_RELATIONSHIP($,$,#5602,#5601)
REPRESENTATION_RELATIONSHIP_WITH_TRANSFORMATION(#39)
SHAPE_REPRESENTATION_RELATIONSHIP()
);
#65=(
REPRESENTATION_RELATIONSHIP($,$,#5615,#5601)
REPRESENTATION_RELATIONSHIP_WITH_TRANSFORMATION(#40)
SHAPE_REPRESENTATION_RELATIONSHIP()
);
#66=CONTEXT_DEPENDENT_SHAPE_REPRESENTATION(#41,#5567);
#67=CONTEXT_DEPENDENT_SHAPE_REPRESENTATION(#42,#5568);
#68=CONTEXT_DEPENDENT_SHAPE_REPRESENTATION(#43,#5569);
#69=CONTEXT_DEPENDENT_SHAPE_REPRESENTATION(#44,#5570);
#70=CONTEXT_DEPENDENT_SHAPE_REPRESENTATION(#45,#5571);
#71=CONTEXT_DEPENDENT_SHAPE_REPRESENTATION(#46,#5577);
#72=CONTEXT_DEPENDENT_SHAPE_REPRESENTATION(#47,#5578);
#73=CONTEXT_DEPENDENT_SHAPE_REPRESENTATION(#48,#5579);
#74=CONTEXT_DEPENDENT_SHAPE_REPRESENTATION(#49,#5580);
#75=CONTEXT_DEPENDENT_SHAPE_REPRESENTATION(#50,#5581);
#76=CONTEXT_DEPENDENT_SHAPE_REPRESENTATION(#51,#5582);
#77=CONTEXT_DEPENDENT_SHAPE_REPRESENTATION(#52,#5583);
#78=CONTEXT_DEPENDENT_SHAPE_REPRESENTATION(#53,#5584);
#79=CONTEXT_DEPENDENT_SHAPE_REPRESENTATION(#54,#5585);
#80=CONTEXT_DEPENDENT_SHAPE_REPRESENTATION(#55,#5586);
#81=CONTEXT_DEPENDENT_SHAPE_REPRESENTATION(#56,#5587);
#82=CONTEXT_DEPENDENT_SHAPE_REPRESENTATION(#57,#5588);
#83=CONTEXT_DEPENDENT_SHAPE_REPRESENTATION(#58,#5589);
#84=CONTEXT_DEPENDENT_SHAPE_REPRESENTATION(#59,#5590);
#85=CONTEXT_DEPENDENT_SHAPE_REPRESENTATION(#60,#5591);
#86=CONTEXT_DEPENDENT_SHAPE_REPRESENTATION(#61,#5596);
#87=CONTEXT_DEPENDENT_SHAPE_REPRESENTATION(#62,#5597);
#88=CONTEXT_DEPENDENT_SHAPE_REPRESENTATION(#63,#5598);
#89=CONTEXT_DEPENDENT_SHAPE_REPRESENTATION(#64,#5599);
#90=CONTEXT_DEPENDENT_SHAPE_REPRESENTATION(#65,#5600);
#91=NEXT_ASSEMBLY_USAGE_OCCURRENCE('Inner ring:1','Inner ring:1',
'Inner ring:1',#5623,#5624,'Inner ring:1');
#92=NEXT_ASSEMBLY_USAGE_OCCURRENCE('Outer ring:1','Outer ring:1',
'Outer ring:1',#5623,#5625,'Outer ring:1');
#93=NEXT_ASSEMBLY_USAGE_OCCURRENCE('Balls:1','Balls:1','Balls:1',#5623,
#5626,'Balls:1');
#94=NEXT_ASSEMBLY_USAGE_OCCURRENCE('Cage:1','Cage:1','Cage:1',#5623,#5627,
'Cage:1');
#95=NEXT_ASSEMBLY_USAGE_OCCURRENCE('Seals 2RS:1','Seals 2RS:1',
'Seals 2RS:1',#5623,#5628,'Seals 2RS:1');
#96=NEXT_ASSEMBLY_USAGE_OCCURRENCE('Flanged housing:1',
'Flanged housing:1','Flanged housing:1',#5621,#5622,'Flanged housing:1');
#97=NEXT_ASSEMBLY_USAGE_OCCURRENCE(
'Sealed Ball Bearing - 20 x 47 x 14 mm:2',
'Sealed Ball Bearing - 20 x 47 x 14 mm:2',
'Sealed Ball Bearing - 20 x 47 x 14 mm:2',#5621,#5623,
'Sealed Ball Bearing - 20 x 47 x 14 mm:2');
#98=NEXT_ASSEMBLY_USAGE_OCCURRENCE(
'Sealed Ball Bearing - 20 x 47 x 14 mm:3',
'Sealed Ball Bearing - 20 x 47 x 14 mm:3',
'Sealed Ball Bearing - 20 x 47 x 14 mm:3',#5621,#5623,
'Sealed Ball Bearing - 20 x 47 x 14 mm:3');
#99=NEXT_ASSEMBLY_USAGE_OCCURRENCE('Outer race spacer:2',
'Outer race spacer:2','Outer race spacer:2',#5621,#5629,
'Outer race spacer:2');
#100=NEXT_ASSEMBLY_USAGE_OCCURRENCE('Seal cap:2','Seal cap:2',
'Seal cap:2',#5621,#5630,'Seal cap:2');
#101=NEXT_ASSEMBLY_USAGE_OCCURRENCE('Dust seal envelope:2',
'Dust seal envelope:2','Dust seal envelope:2',#5621,#5631,
'Dust seal envelope:2');
#102=NEXT_ASSEMBLY_USAGE_OCCURRENCE('Rear cap:2','Rear cap:2',
'Rear cap:2',#5621,#5632,'Rear cap:2');
#103=NEXT_ASSEMBLY_USAGE_OCCURRENCE('Cap Screw - M4x16:2',
'Cap Screw - M4x16:2','Cap Screw - M4x16:2',#5621,#5633,
'Cap Screw - M4x16:2');
#104=NEXT_ASSEMBLY_USAGE_OCCURRENCE('Cap Screw - M4x16:3',
'Cap Screw - M4x16:3','Cap Screw - M4x16:3',#5621,#5633,
'Cap Screw - M4x16:3');
#105=NEXT_ASSEMBLY_USAGE_OCCURRENCE('Cap Screw - M4x16:4',
'Cap Screw - M4x16:4','Cap Screw - M4x16:4',#5621,#5633,
'Cap Screw - M4x16:4');
#106=NEXT_ASSEMBLY_USAGE_OCCURRENCE('Cap Screw - M4x16:5',
'Cap Screw - M4x16:5','Cap Screw - M4x16:5',#5621,#5633,
'Cap Screw - M4x16:5');
#107=NEXT_ASSEMBLY_USAGE_OCCURRENCE('Cap Screw - M4x16:6',
'Cap Screw - M4x16:6','Cap Screw - M4x16:6',#5621,#5633,
'Cap Screw - M4x16:6');
#108=NEXT_ASSEMBLY_USAGE_OCCURRENCE('Cap Screw - M4x16:7',
'Cap Screw - M4x16:7','Cap Screw - M4x16:7',#5621,#5633,
'Cap Screw - M4x16:7');
#109=NEXT_ASSEMBLY_USAGE_OCCURRENCE('Cap Screw - M4x16:8',
'Cap Screw - M4x16:8','Cap Screw - M4x16:8',#5621,#5633,
'Cap Screw - M4x16:8');
#110=NEXT_ASSEMBLY_USAGE_OCCURRENCE('Cap Screw - M4x16:9',
'Cap Screw - M4x16:9','Cap Screw - M4x16:9',#5621,#5633,
'Cap Screw - M4x16:9');
#111=NEXT_ASSEMBLY_USAGE_OCCURRENCE('Retained shaft:1',
'Retained shaft:1','Retained shaft:1',#5634,#5635,'Retained shaft:1');
#112=NEXT_ASSEMBLY_USAGE_OCCURRENCE('Inner race spacer:2',
'Inner race spacer:2','Inner race spacer:2',#5634,#5636,
'Inner race spacer:2');
#113=NEXT_ASSEMBLY_USAGE_OCCURRENCE('Installed retaining ring:2',
'Installed retaining ring:2','Installed retaining ring:2',#5634,#5637,
'Installed retaining ring:2');
#114=NEXT_ASSEMBLY_USAGE_OCCURRENCE(
'Flanged housing bearings and seal caps:1',
'Flanged housing bearings and seal caps:1',
'Flanged housing bearings and seal caps:1',#5620,#5621,
'Flanged housing bearings and seal caps:1');
#115=NEXT_ASSEMBLY_USAGE_OCCURRENCE('Shaft spacer and retaining ring:1',
'Shaft spacer and retaining ring:1','Shaft spacer and retaining ring:1',
#5620,#5634,'Shaft spacer and retaining ring:1');
#116=B_SPLINE_CURVE_WITH_KNOTS('',3,(#3902,#3903,#3904,#3905,#3906,#3907,
#3908,#3909,#3910,#3911,#3912,#3913,#3914,#3915,#3916,#3917,#3918,#3919,
#3920,#3921,#3922,#3923),.UNSPECIFIED.,.F.,.F.,(4,2,2,2,2,2,2,2,2,2,4),
(0.0789094028588958,0.210573405340968,0.315860108011452,0.421146810681936,
0.522142632548711,0.623138454415485,0.72413427628226,0.825130098149035,
0.930416800819519,1.03570350349,1.16736750597208),.UNSPECIFIED.);
#117=B_SPLINE_CURVE_WITH_KNOTS('',3,(#3927,#3928,#3929,#3930,#3931,#3932,
#3933,#3934,#3935,#3936,#3937,#3938,#3939,#3940,#3941,#3942,#3943,#3944,
#3945,#3946,#3947,#3948),.UNSPECIFIED.,.F.,.F.,(4,2,2,2,2,2,2,2,2,2,4),
(0.0774793363974613,0.142088896491891,0.284177792983782,0.411119756996526,
0.514392970548519,0.617666184100513,0.720939397652506,0.8242126112045,0.951154575217244,
1.09324347170913,1.15785303180356),.UNSPECIFIED.);
#118=B_SPLINE_CURVE_WITH_KNOTS('',3,(#3954,#3955,#3956,#3957,#3958,#3959,
#3960,#3961,#3962,#3963,#3964,#3965,#3966,#3967,#3968,#3969,#3970,#3971,
#3972,#3973,#3974,#3975),.UNSPECIFIED.,.F.,.F.,(4,2,2,2,2,2,2,2,2,2,4),
(0.0774793363974613,0.142088896491891,0.284177792983782,0.411119756996525,
0.514392970548519,0.617666184100513,0.720939397652506,0.8242126112045,0.951154575217243,
1.09324347170913,1.15785303180356),.UNSPECIFIED.);
#119=B_SPLINE_CURVE_WITH_KNOTS('',3,(#3979,#3980,#3981,#3982,#3983,#3984,
#3985,#3986,#3987,#3988,#3989,#3990,#3991,#3992,#3993,#3994,#3995,#3996,
#3997,#3998,#3999,#4000),.UNSPECIFIED.,.F.,.F.,(4,2,2,2,2,2,2,2,2,2,4),
(0.0774793363974614,0.142088896491891,0.284177792983781,0.411119756996525,
0.514392970548519,0.617666184100512,0.720939397652506,0.824212611204499,
0.951154575217243,1.09324347170913,1.15785303180356),.UNSPECIFIED.);
#120=B_SPLINE_CURVE_WITH_KNOTS('',3,(#4004,#4005,#4006,#4007,#4008,#4009,
#4010,#4011,#4012,#4013,#4014,#4015),.UNSPECIFIED.,.F.,.F.,(4,2,2,2,2,4),
(0.0774793363974613,0.142088896491891,0.284177792983781,0.411119756996525,
0.514392970548519,0.617666184100512),.UNSPECIFIED.);
#121=B_SPLINE_CURVE_WITH_KNOTS('',3,(#4020,#4021,#4022,#4023,#4024,#4025,
#4026,#4027,#4028,#4029,#4030,#4031),.UNSPECIFIED.,.F.,.F.,(4,2,2,2,2,4),
(0.617666184100512,0.720939397652506,0.824212611204499,0.951154575217243,
1.09324347170913,1.15785303180356),.UNSPECIFIED.);
#122=B_SPLINE_CURVE_WITH_KNOTS('',3,(#4035,#4036,#4037,#4038,#4039,#4040,
#4041,#4042,#4043,#4044,#4045,#4046,#4047,#4048,#4049,#4050,#4051,#4052,
#4053,#4054,#4055,#4056),.UNSPECIFIED.,.F.,.F.,(4,2,2,2,2,2,2,2,2,2,4),
(0.0774793363974613,0.142088896491891,0.284177792983782,0.411119756996526,
0.514392970548519,0.617666184100513,0.720939397652507,0.8242126112045,0.951154575217245,
1.09324347170914,1.15785303180356),.UNSPECIFIED.);
#123=B_SPLINE_CURVE_WITH_KNOTS('',3,(#4060,#4061,#4062,#4063,#4064,#4065,
#4066,#4067,#4068,#4069,#4070,#4071,#4072,#4073,#4074,#4075,#4076,#4077,
#4078,#4079,#4080,#4081),.UNSPECIFIED.,.F.,.F.,(4,2,2,2,2,2,2,2,2,2,4),
(0.0774793363974613,0.142088896491891,0.284177792983782,0.411119756996526,
0.514392970548519,0.617666184100513,0.720939397652506,0.824212611204499,
0.951154575217243,1.09324347170913,1.15785303180356),.UNSPECIFIED.);
#124=B_SPLINE_CURVE_WITH_KNOTS('',3,(#4085,#4086,#4087,#4088,#4089,#4090,
#4091,#4092,#4093,#4094,#4095,#4096,#4097,#4098,#4099,#4100,#4101,#4102,
#4103,#4104,#4105,#4106),.UNSPECIFIED.,.F.,.F.,(4,2,2,2,2,2,2,2,2,2,4),
(0.0774793363974613,0.142088896491891,0.284177792983782,0.411119756996526,
0.514392970548519,0.617666184100513,0.720939397652506,0.8242126112045,0.951154575217244,
1.09324347170913,1.15785303180356),.UNSPECIFIED.);
#125=B_SPLINE_CURVE_WITH_KNOTS('',3,(#4110,#4111,#4112,#4113,#4114,#4115,
#4116,#4117,#4118,#4119,#4120,#4121,#4122,#4123,#4124,#4125,#4126,#4127,
#4128,#4129,#4130,#4131),.UNSPECIFIED.,.F.,.F.,(4,2,2,2,2,2,2,2,2,2,4),
(0.0774793363974613,0.142088896491891,0.284177792983782,0.411119756996526,
0.514392970548519,0.617666184100513,0.720939397652506,0.8242126112045,0.951154575217243,
1.09324347170913,1.15785303180356),.UNSPECIFIED.);
#126=B_SPLINE_CURVE_WITH_KNOTS('',3,(#4139,#4140,#4141,#4142,#4143,#4144,
#4145,#4146,#4147,#4148,#4149,#4150,#4151,#4152,#4153,#4154,#4155,#4156,
#4157,#4158,#4159,#4160),.UNSPECIFIED.,.F.,.F.,(4,2,2,2,2,2,2,2,2,2,4),
(0.0789094028588958,0.210573405340968,0.315860108011452,0.421146810681936,
0.522142632548711,0.623138454415485,0.72413427628226,0.825130098149035,
0.930416800819519,1.03570350349,1.16736750597208),.UNSPECIFIED.);
#127=B_SPLINE_CURVE_WITH_KNOTS('',3,(#4168,#4169,#4170,#4171,#4172,#4173,
#4174,#4175,#4176,#4177,#4178,#4179,#4180,#4181,#4182,#4183,#4184,#4185,
#4186,#4187,#4188,#4189),.UNSPECIFIED.,.F.,.F.,(4,2,2,2,2,2,2,2,2,2,4),
(0.0789094028588958,0.210573405340969,0.315860108011453,0.421146810681937,
0.522142632548712,0.623138454415486,0.724134276282261,0.825130098149035,
0.930416800819519,1.03570350349,1.16736750597208),.UNSPECIFIED.);
#128=B_SPLINE_CURVE_WITH_KNOTS('',3,(#4198,#4199,#4200,#4201,#4202,#4203,
#4204,#4205,#4206,#4207,#4208,#4209),.UNSPECIFIED.,.F.,.F.,(4,2,2,2,2,4),
(0.0789094028588958,0.210573405340968,0.315860108011452,0.421146810681937,
0.522142632548711,0.623138454415486),.UNSPECIFIED.);
#129=B_SPLINE_CURVE_WITH_KNOTS('',3,(#4211,#4212,#4213,#4214,#4215,#4216,
#4217,#4218,#4219,#4220,#4221,#4222),.UNSPECIFIED.,.F.,.F.,(4,2,2,2,2,4),
(0.623138454415486,0.72413427628226,0.825130098149035,0.930416800819519,
1.03570350349,1.16736750597208),.UNSPECIFIED.);
#130=B_SPLINE_CURVE_WITH_KNOTS('',3,(#4229,#4230,#4231,#4232,#4233,#4234,
#4235,#4236,#4237,#4238,#4239,#4240,#4241,#4242,#4243,#4244,#4245,#4246,
#4247,#4248,#4249,#4250),.UNSPECIFIED.,.F.,.F.,(4,2,2,2,2,2,2,2,2,2,4),
(0.0789094028588958,0.210573405340968,0.315860108011452,0.421146810681936,
0.522142632548711,0.623138454415486,0.72413427628226,0.825130098149035,
0.930416800819519,1.03570350349,1.16736750597208),.UNSPECIFIED.);
#131=B_SPLINE_CURVE_WITH_KNOTS('',3,(#4258,#4259,#4260,#4261,#4262,#4263,
#4264,#4265,#4266,#4267,#4268,#4269,#4270,#4271,#4272,#4273,#4274,#4275,
#4276,#4277,#4278,#4279),.UNSPECIFIED.,.F.,.F.,(4,2,2,2,2,2,2,2,2,2,4),
(0.0789094028588957,0.210573405340968,0.315860108011452,0.421146810681936,
0.522142632548711,0.623138454415485,0.72413427628226,0.825130098149035,
0.930416800819519,1.03570350349,1.16736750597207),.UNSPECIFIED.);
#132=B_SPLINE_CURVE_WITH_KNOTS('',3,(#4287,#4288,#4289,#4290,#4291,#4292,
#4293,#4294,#4295,#4296,#4297,#4298,#4299,#4300,#4301,#4302,#4303,#4304,
#4305,#4306,#4307,#4308),.UNSPECIFIED.,.F.,.F.,(4,2,2,2,2,2,2,2,2,2,4),
(0.0789094028588958,0.210573405340968,0.315860108011452,0.421146810681936,
0.522142632548711,0.623138454415486,0.72413427628226,0.825130098149035,
0.930416800819519,1.03570350349,1.16736750597208),.UNSPECIFIED.);
#133=B_SPLINE_CURVE_WITH_KNOTS('',3,(#4317,#4318,#4319,#4320,#4321,#4322,
#4323,#4324,#4325,#4326,#4327,#4328,#4329,#4330,#4331,#4332,#4333,#4334,
#4335,#4336,#4337,#4338),.UNSPECIFIED.,.F.,.F.,(4,2,2,2,2,2,2,2,2,2,4),
(0.0789094028588958,0.210573405340968,0.315860108011452,0.421146810681936,
0.522142632548711,0.623138454415485,0.72413427628226,0.825130098149035,
0.930416800819519,1.03570350349,1.16736750597208),.UNSPECIFIED.);
#134=B_SPLINE_CURVE_WITH_KNOTS('',3,(#4661,#4662,#4663,#4664,#4665,#4666),
 .UNSPECIFIED.,.F.,.F.,(4,2,4),(-0.12,-0.06,0.),.UNSPECIFIED.);
#135=B_SPLINE_CURVE_WITH_KNOTS('',3,(#4881,#4882,#4883,#4884,#4885,#4886),
 .UNSPECIFIED.,.F.,.F.,(4,2,4),(-0.12,-0.06,0.),.UNSPECIFIED.);
#136=SPHERICAL_SURFACE('',#2607,0.3969);
#137=SPHERICAL_SURFACE('',#2609,0.3969);
#138=SPHERICAL_SURFACE('',#2611,0.3969);
#139=SPHERICAL_SURFACE('',#2613,0.3969);
#140=SPHERICAL_SURFACE('',#2615,0.3969);
#141=SPHERICAL_SURFACE('',#2617,0.3969);
#142=SPHERICAL_SURFACE('',#2619,0.3969);
#143=SPHERICAL_SURFACE('',#2621,0.3969);
#144=SPHERICAL_SURFACE('',#2624,0.412776);
#145=SPHERICAL_SURFACE('',#2640,0.412776);
#146=SPHERICAL_SURFACE('',#2645,0.412776);
#147=SPHERICAL_SURFACE('',#2650,0.412776);
#148=SPHERICAL_SURFACE('',#2655,0.412776);
#149=SPHERICAL_SURFACE('',#2660,0.412776);
#150=SPHERICAL_SURFACE('',#2665,0.412776);
#151=SPHERICAL_SURFACE('',#2673,0.412776);
#152=CONICAL_SURFACE('',#2578,1.05,0.785398163397449);
#153=CONICAL_SURFACE('',#2585,1.05,0.785398163397449);
#154=CONICAL_SURFACE('',#2598,2.3,0.785398163397449);
#155=CONICAL_SURFACE('',#2602,2.3,0.785398163397449);
#156=CONICAL_SURFACE('',#2774,0.325,0.785398163397448);
#157=CONICAL_SURFACE('',#2778,0.335,0.785398163397448);
#158=CONICAL_SURFACE('',#2782,0.21,0.463647609000806);
#159=CONICAL_SURFACE('',#2786,0.18,0.785398163397448);
#160=TOROIDAL_SURFACE('',#2567,1.675,0.412776);
#161=TOROIDAL_SURFACE('',#2587,1.675,0.412776);
#162=SHAPE_REPRESENTATION_RELATIONSHIP('SRR','None',#5603,#176);
#163=SHAPE_REPRESENTATION_RELATIONSHIP('SRR','None',#5605,#177);
#164=SHAPE_REPRESENTATION_RELATIONSHIP('SRR','None',#5606,#178);
#165=SHAPE_REPRESENTATION_RELATIONSHIP('SRR','None',#5607,#179);
#166=SHAPE_REPRESENTATION_RELATIONSHIP('SRR','None',#5608,#180);
#167=SHAPE_REPRESENTATION_RELATIONSHIP('SRR','None',#5609,#181);
#168=SHAPE_REPRESENTATION_RELATIONSHIP('SRR','None',#5610,#182);
#169=SHAPE_REPRESENTATION_RELATIONSHIP('SRR','None',#5611,#183);
#170=SHAPE_REPRESENTATION_RELATIONSHIP('SRR','None',#5612,#184);
#171=SHAPE_REPRESENTATION_RELATIONSHIP('SRR','None',#5613,#185);
#172=SHAPE_REPRESENTATION_RELATIONSHIP('SRR','None',#5614,#186);
#173=SHAPE_REPRESENTATION_RELATIONSHIP('SRR','None',#5616,#187);
#174=SHAPE_REPRESENTATION_RELATIONSHIP('SRR','None',#5617,#188);
#175=SHAPE_REPRESENTATION_RELATIONSHIP('SRR','None',#5618,#189);
#176=ADVANCED_BREP_SHAPE_REPRESENTATION('',(#212),#5519);
#177=ADVANCED_BREP_SHAPE_REPRESENTATION('',(#213),#5521);
#178=ADVANCED_BREP_SHAPE_REPRESENTATION('',(#214),#5522);
#179=ADVANCED_BREP_SHAPE_REPRESENTATION('',(#215,#216,#217,#218,#219,#220,
#221,#222),#5523);
#180=ADVANCED_BREP_SHAPE_REPRESENTATION('',(#223),#5524);
#181=ADVANCED_BREP_SHAPE_REPRESENTATION('',(#224,#225),#5525);
#182=ADVANCED_BREP_SHAPE_REPRESENTATION('',(#226),#5526);
#183=ADVANCED_BREP_SHAPE_REPRESENTATION('',(#227),#5527);
#184=ADVANCED_BREP_SHAPE_REPRESENTATION('',(#228),#5528);
#185=ADVANCED_BREP_SHAPE_REPRESENTATION('',(#229),#5529);
#186=ADVANCED_BREP_SHAPE_REPRESENTATION('',(#15),#5530);
#187=ADVANCED_BREP_SHAPE_REPRESENTATION('',(#230),#5532);
#188=ADVANCED_BREP_SHAPE_REPRESENTATION('',(#231),#5533);
#189=ADVANCED_BREP_SHAPE_REPRESENTATION('',(#232),#5534);
#190=STYLED_ITEM('',(#5743),#212);
#191=STYLED_ITEM('',(#5764),#213);
#192=STYLED_ITEM('',(#5764),#214);
#193=STYLED_ITEM('',(#5764),#215);
#194=STYLED_ITEM('',(#5764),#216);
#195=STYLED_ITEM('',(#5764),#217);
#196=STYLED_ITEM('',(#5764),#218);
#197=STYLED_ITEM('',(#5764),#219);
#198=STYLED_ITEM('',(#5764),#220);
#199=STYLED_ITEM('',(#5764),#221);
#200=STYLED_ITEM('',(#5764),#222);
#201=STYLED_ITEM('',(#5764),#223);
#202=STYLED_ITEM('',(#5764),#224);
#203=STYLED_ITEM('',(#5764),#225);
#204=STYLED_ITEM('',(#5764),#226);
#205=STYLED_ITEM('',(#5771),#227);
#206=STYLED_ITEM('',(#5771),#228);
#207=STYLED_ITEM('',(#5757),#229);
#208=STYLED_ITEM('',(#5771),#15);
#209=STYLED_ITEM('',(#5764),#230);
#210=STYLED_ITEM('',(#5764),#231);
#211=STYLED_ITEM('',(#5778),#232);
#212=MANIFOLD_SOLID_BREP('Body1',#2324);
#213=MANIFOLD_SOLID_BREP('Body1',#2325);
#214=MANIFOLD_SOLID_BREP('Body1',#2326);
#215=MANIFOLD_SOLID_BREP('Body1',#2327);
#216=MANIFOLD_SOLID_BREP('Body2',#2328);
#217=MANIFOLD_SOLID_BREP('Body3',#2329);
#218=MANIFOLD_SOLID_BREP('Body4',#2330);
#219=MANIFOLD_SOLID_BREP('Body5',#2331);
#220=MANIFOLD_SOLID_BREP('Body6',#2332);
#221=MANIFOLD_SOLID_BREP('Body7',#2333);
#222=MANIFOLD_SOLID_BREP('Body8',#2334);
#223=MANIFOLD_SOLID_BREP('Continuous crown cage',#2335);
#224=MANIFOLD_SOLID_BREP('Body1',#2336);
#225=MANIFOLD_SOLID_BREP('Body2',#2337);
#226=MANIFOLD_SOLID_BREP('Body1',#2338);
#227=MANIFOLD_SOLID_BREP('Body1',#2339);
#228=MANIFOLD_SOLID_BREP('Body1',#2340);
#229=MANIFOLD_SOLID_BREP('Body1',#2341);
#230=MANIFOLD_SOLID_BREP('Body1',#2344);
#231=MANIFOLD_SOLID_BREP('Body1',#2345);
#232=MANIFOLD_SOLID_BREP('Body1',#2346);
#233=FACE_BOUND('',#531,.T.);
#234=FACE_BOUND('',#532,.T.);
#235=FACE_BOUND('',#533,.T.);
#236=FACE_BOUND('',#534,.T.);
#237=FACE_BOUND('',#535,.T.);
#238=FACE_BOUND('',#537,.T.);
#239=FACE_BOUND('',#538,.T.);
#240=FACE_BOUND('',#539,.T.);
#241=FACE_BOUND('',#540,.T.);
#242=FACE_BOUND('',#541,.T.);
#243=FACE_BOUND('',#547,.T.);
#244=FACE_BOUND('',#548,.T.);
#245=FACE_BOUND('',#549,.T.);
#246=FACE_BOUND('',#550,.T.);
#247=FACE_BOUND('',#551,.T.);
#248=FACE_BOUND('',#553,.T.);
#249=FACE_BOUND('',#554,.T.);
#250=FACE_BOUND('',#555,.T.);
#251=FACE_BOUND('',#556,.T.);
#252=FACE_BOUND('',#557,.T.);
#253=FACE_BOUND('',#563,.T.);
#254=FACE_BOUND('',#566,.T.);
#255=FACE_BOUND('',#571,.T.);
#256=FACE_BOUND('',#576,.T.);
#257=FACE_BOUND('',#604,.T.);
#258=FACE_BOUND('',#607,.T.);
#259=FACE_BOUND('',#610,.T.);
#260=FACE_BOUND('',#613,.T.);
#261=FACE_BOUND('',#616,.T.);
#262=FACE_BOUND('',#621,.T.);
#263=FACE_BOUND('',#623,.T.);
#264=FACE_BOUND('',#630,.T.);
#265=FACE_BOUND('',#633,.T.);
#266=FACE_BOUND('',#637,.T.);
#267=FACE_BOUND('',#638,.T.);
#268=FACE_BOUND('',#639,.T.);
#269=FACE_BOUND('',#640,.T.);
#270=FACE_BOUND('',#641,.T.);
#271=FACE_BOUND('',#643,.T.);
#272=FACE_BOUND('',#644,.T.);
#273=FACE_BOUND('',#645,.T.);
#274=FACE_BOUND('',#646,.T.);
#275=FACE_BOUND('',#647,.T.);
#276=FACE_BOUND('',#651,.T.);
#277=FACE_BOUND('',#653,.T.);
#278=FACE_BOUND('',#660,.T.);
#279=FACE_BOUND('',#664,.T.);
#280=FACE_BOUND('',#665,.T.);
#281=FACE_BOUND('',#666,.T.);
#282=FACE_BOUND('',#667,.T.);
#283=FACE_BOUND('',#668,.T.);
#284=FACE_BOUND('',#670,.T.);
#285=FACE_BOUND('',#671,.T.);
#286=FACE_BOUND('',#672,.T.);
#287=FACE_BOUND('',#673,.T.);
#288=FACE_BOUND('',#674,.T.);
#289=FACE_BOUND('',#680,.T.);
#290=FACE_BOUND('',#695,.T.);
#291=FACE_BOUND('',#697,.T.);
#292=FACE_BOUND('',#700,.T.);
#293=FACE_BOUND('',#702,.T.);
#294=FACE_BOUND('',#711,.T.);
#295=FACE_BOUND('',#713,.T.);
#296=FACE_BOUND('',#717,.T.);
#297=FACE_BOUND('',#718,.T.);
#298=FACE_BOUND('',#724,.T.);
#299=FACE_BOUND('',#725,.T.);
#300=PLANE('',#2520);
#301=PLANE('',#2524);
#302=PLANE('',#2528);
#303=PLANE('',#2532);
#304=PLANE('',#2536);
#305=PLANE('',#2540);
#306=PLANE('',#2544);
#307=PLANE('',#2548);
#308=PLANE('',#2549);
#309=PLANE('',#2552);
#310=PLANE('',#2563);
#311=PLANE('',#2564);
#312=PLANE('',#2580);
#313=PLANE('',#2583);
#314=PLANE('',#2595);
#315=PLANE('',#2604);
#316=PLANE('',#2637);
#317=PLANE('',#2642);
#318=PLANE('',#2647);
#319=PLANE('',#2652);
#320=PLANE('',#2657);
#321=PLANE('',#2662);
#322=PLANE('',#2671);
#323=PLANE('',#2675);
#324=PLANE('',#2676);
#325=PLANE('',#2678);
#326=PLANE('',#2683);
#327=PLANE('',#2686);
#328=PLANE('',#2691);
#329=PLANE('',#2706);
#330=PLANE('',#2707);
#331=PLANE('',#2724);
#332=PLANE('',#2729);
#333=PLANE('',#2735);
#334=PLANE('',#2736);
#335=PLANE('',#2744);
#336=PLANE('',#2745);
#337=PLANE('',#2762);
#338=PLANE('',#2769);
#339=PLANE('',#2770);
#340=PLANE('',#2772);
#341=PLANE('',#2780);
#342=PLANE('',#2788);
#343=PLANE('',#2789);
#344=PLANE('',#2790);
#345=PLANE('',#2791);
#346=PLANE('',#2792);
#347=PLANE('',#2793);
#348=PLANE('',#2794);
#349=PLANE('',#2795);
#350=PLANE('',#2796);
#351=PLANE('',#2817);
#352=PLANE('',#2819);
#353=PLANE('',#2823);
#354=PLANE('',#2825);
#355=PLANE('',#2833);
#356=PLANE('',#2834);
#357=PLANE('',#2842);
#358=PLANE('',#2843);
#359=PLANE('',#2851);
#360=PLANE('',#2861);
#361=FACE_OUTER_BOUND('',#510,.T.);
#362=FACE_OUTER_BOUND('',#511,.T.);
#363=FACE_OUTER_BOUND('',#512,.T.);
#364=FACE_OUTER_BOUND('',#513,.T.);
#365=FACE_OUTER_BOUND('',#514,.T.);
#366=FACE_OUTER_BOUND('',#515,.T.);
#367=FACE_OUTER_BOUND('',#516,.T.);
#368=FACE_OUTER_BOUND('',#517,.T.);
#369=FACE_OUTER_BOUND('',#518,.T.);
#370=FACE_OUTER_BOUND('',#519,.T.);
#371=FACE_OUTER_BOUND('',#520,.T.);
#372=FACE_OUTER_BOUND('',#521,.T.);
#373=FACE_OUTER_BOUND('',#522,.T.);
#374=FACE_OUTER_BOUND('',#523,.T.);
#375=FACE_OUTER_BOUND('',#524,.T.);
#376=FACE_OUTER_BOUND('',#525,.T.);
#377=FACE_OUTER_BOUND('',#526,.T.);
#378=FACE_OUTER_BOUND('',#527,.T.);
#379=FACE_OUTER_BOUND('',#528,.T.);
#380=FACE_OUTER_BOUND('',#529,.T.);
#381=FACE_OUTER_BOUND('',#530,.T.);
#382=FACE_OUTER_BOUND('',#536,.T.);
#383=FACE_OUTER_BOUND('',#542,.T.);
#384=FACE_OUTER_BOUND('',#543,.T.);
#385=FACE_OUTER_BOUND('',#544,.T.);
#386=FACE_OUTER_BOUND('',#545,.T.);
#387=FACE_OUTER_BOUND('',#546,.T.);
#388=FACE_OUTER_BOUND('',#552,.T.);
#389=FACE_OUTER_BOUND('',#558,.T.);
#390=FACE_OUTER_BOUND('',#559,.T.);
#391=FACE_OUTER_BOUND('',#560,.T.);
#392=FACE_OUTER_BOUND('',#561,.T.);
#393=FACE_OUTER_BOUND('',#562,.T.);
#394=FACE_OUTER_BOUND('',#564,.T.);
#395=FACE_OUTER_BOUND('',#565,.T.);
#396=FACE_OUTER_BOUND('',#567,.T.);
#397=FACE_OUTER_BOUND('',#568,.T.);
#398=FACE_OUTER_BOUND('',#569,.T.);
#399=FACE_OUTER_BOUND('',#570,.T.);
#400=FACE_OUTER_BOUND('',#572,.T.);
#401=FACE_OUTER_BOUND('',#573,.T.);
#402=FACE_OUTER_BOUND('',#574,.T.);
#403=FACE_OUTER_BOUND('',#575,.T.);
#404=FACE_OUTER_BOUND('',#577,.T.);
#405=FACE_OUTER_BOUND('',#578,.T.);
#406=FACE_OUTER_BOUND('',#579,.T.);
#407=FACE_OUTER_BOUND('',#580,.T.);
#408=FACE_OUTER_BOUND('',#581,.T.);
#409=FACE_OUTER_BOUND('',#582,.T.);
#410=FACE_OUTER_BOUND('',#583,.T.);
#411=FACE_OUTER_BOUND('',#584,.T.);
#412=FACE_OUTER_BOUND('',#585,.T.);
#413=FACE_OUTER_BOUND('',#586,.T.);
#414=FACE_OUTER_BOUND('',#587,.T.);
#415=FACE_OUTER_BOUND('',#588,.T.);
#416=FACE_OUTER_BOUND('',#589,.T.);
#417=FACE_OUTER_BOUND('',#590,.T.);
#418=FACE_OUTER_BOUND('',#591,.T.);
#419=FACE_OUTER_BOUND('',#592,.T.);
#420=FACE_OUTER_BOUND('',#593,.T.);
#421=FACE_OUTER_BOUND('',#594,.T.);
#422=FACE_OUTER_BOUND('',#595,.T.);
#423=FACE_OUTER_BOUND('',#596,.T.);
#424=FACE_OUTER_BOUND('',#597,.T.);
#425=FACE_OUTER_BOUND('',#598,.T.);
#426=FACE_OUTER_BOUND('',#599,.T.);
#427=FACE_OUTER_BOUND('',#600,.T.);
#428=FACE_OUTER_BOUND('',#601,.T.);
#429=FACE_OUTER_BOUND('',#602,.T.);
#430=FACE_OUTER_BOUND('',#603,.T.);
#431=FACE_OUTER_BOUND('',#605,.T.);
#432=FACE_OUTER_BOUND('',#606,.T.);
#433=FACE_OUTER_BOUND('',#608,.T.);
#434=FACE_OUTER_BOUND('',#609,.T.);
#435=FACE_OUTER_BOUND('',#611,.T.);
#436=FACE_OUTER_BOUND('',#612,.T.);
#437=FACE_OUTER_BOUND('',#614,.T.);
#438=FACE_OUTER_BOUND('',#615,.T.);
#439=FACE_OUTER_BOUND('',#617,.T.);
#440=FACE_OUTER_BOUND('',#618,.T.);
#441=FACE_OUTER_BOUND('',#619,.T.);
#442=FACE_OUTER_BOUND('',#620,.T.);
#443=FACE_OUTER_BOUND('',#622,.T.);
#444=FACE_OUTER_BOUND('',#624,.T.);
#445=FACE_OUTER_BOUND('',#625,.T.);
#446=FACE_OUTER_BOUND('',#626,.T.);
#447=FACE_OUTER_BOUND('',#627,.T.);
#448=FACE_OUTER_BOUND('',#628,.T.);
#449=FACE_OUTER_BOUND('',#629,.T.);
#450=FACE_OUTER_BOUND('',#631,.T.);
#451=FACE_OUTER_BOUND('',#632,.T.);
#452=FACE_OUTER_BOUND('',#634,.T.);
#453=FACE_OUTER_BOUND('',#635,.T.);
#454=FACE_OUTER_BOUND('',#636,.T.);
#455=FACE_OUTER_BOUND('',#642,.T.);
#456=FACE_OUTER_BOUND('',#648,.T.);
#457=FACE_OUTER_BOUND('',#649,.T.);
#458=FACE_OUTER_BOUND('',#650,.T.);
#459=FACE_OUTER_BOUND('',#652,.T.);
#460=FACE_OUTER_BOUND('',#654,.T.);
#461=FACE_OUTER_BOUND('',#655,.T.);
#462=FACE_OUTER_BOUND('',#656,.T.);
#463=FACE_OUTER_BOUND('',#657,.T.);
#464=FACE_OUTER_BOUND('',#658,.T.);
#465=FACE_OUTER_BOUND('',#659,.T.);
#466=FACE_OUTER_BOUND('',#661,.T.);
#467=FACE_OUTER_BOUND('',#662,.T.);
#468=FACE_OUTER_BOUND('',#663,.T.);
#469=FACE_OUTER_BOUND('',#669,.T.);
#470=FACE_OUTER_BOUND('',#675,.T.);
#471=FACE_OUTER_BOUND('',#676,.T.);
#472=FACE_OUTER_BOUND('',#677,.T.);
#473=FACE_OUTER_BOUND('',#678,.T.);
#474=FACE_OUTER_BOUND('',#679,.T.);
#475=FACE_OUTER_BOUND('',#681,.T.);
#476=FACE_OUTER_BOUND('',#682,.T.);
#477=FACE_OUTER_BOUND('',#683,.T.);
#478=FACE_OUTER_BOUND('',#684,.T.);
#479=FACE_OUTER_BOUND('',#685,.T.);
#480=FACE_OUTER_BOUND('',#686,.T.);
#481=FACE_OUTER_BOUND('',#687,.T.);
#482=FACE_OUTER_BOUND('',#688,.T.);
#483=FACE_OUTER_BOUND('',#689,.T.);
#484=FACE_OUTER_BOUND('',#690,.T.);
#485=FACE_OUTER_BOUND('',#691,.T.);
#486=FACE_OUTER_BOUND('',#692,.T.);
#487=FACE_OUTER_BOUND('',#693,.T.);
#488=FACE_OUTER_BOUND('',#694,.T.);
#489=FACE_OUTER_BOUND('',#696,.T.);
#490=FACE_OUTER_BOUND('',#698,.T.);
#491=FACE_OUTER_BOUND('',#699,.T.);
#492=FACE_OUTER_BOUND('',#701,.T.);
#493=FACE_OUTER_BOUND('',#703,.T.);
#494=FACE_OUTER_BOUND('',#704,.T.);
#495=FACE_OUTER_BOUND('',#705,.T.);
#496=FACE_OUTER_BOUND('',#706,.T.);
#497=FACE_OUTER_BOUND('',#707,.T.);
#498=FACE_OUTER_BOUND('',#708,.T.);
#499=FACE_OUTER_BOUND('',#709,.T.);
#500=FACE_OUTER_BOUND('',#710,.T.);
#501=FACE_OUTER_BOUND('',#712,.T.);
#502=FACE_OUTER_BOUND('',#714,.T.);
#503=FACE_OUTER_BOUND('',#715,.T.);
#504=FACE_OUTER_BOUND('',#716,.T.);
#505=FACE_OUTER_BOUND('',#719,.T.);
#506=FACE_OUTER_BOUND('',#720,.T.);
#507=FACE_OUTER_BOUND('',#721,.T.);
#508=FACE_OUTER_BOUND('',#722,.T.);
#509=FACE_OUTER_BOUND('',#723,.T.);
#510=EDGE_LOOP('',(#1550,#1551,#1552,#1553));
#511=EDGE_LOOP('',(#1554,#1555,#1556,#1557));
#512=EDGE_LOOP('',(#1558,#1559,#1560,#1561));
#513=EDGE_LOOP('',(#1562,#1563,#1564,#1565));
#514=EDGE_LOOP('',(#1566,#1567,#1568,#1569));
#515=EDGE_LOOP('',(#1570));
#516=EDGE_LOOP('',(#1571,#1572,#1573,#1574));
#517=EDGE_LOOP('',(#1575));
#518=EDGE_LOOP('',(#1576,#1577,#1578,#1579));
#519=EDGE_LOOP('',(#1580));
#520=EDGE_LOOP('',(#1581,#1582,#1583,#1584));
#521=EDGE_LOOP('',(#1585));
#522=EDGE_LOOP('',(#1586,#1587,#1588,#1589));
#523=EDGE_LOOP('',(#1590));
#524=EDGE_LOOP('',(#1591,#1592,#1593,#1594));
#525=EDGE_LOOP('',(#1595));
#526=EDGE_LOOP('',(#1596,#1597,#1598,#1599));
#527=EDGE_LOOP('',(#1600));
#528=EDGE_LOOP('',(#1601,#1602,#1603,#1604));
#529=EDGE_LOOP('',(#1605));
#530=EDGE_LOOP('',(#1606));
#531=EDGE_LOOP('',(#1607));
#532=EDGE_LOOP('',(#1608));
#533=EDGE_LOOP('',(#1609));
#534=EDGE_LOOP('',(#1610));
#535=EDGE_LOOP('',(#1611));
#536=EDGE_LOOP('',(#1612));
#537=EDGE_LOOP('',(#1613));
#538=EDGE_LOOP('',(#1614));
#539=EDGE_LOOP('',(#1615));
#540=EDGE_LOOP('',(#1616));
#541=EDGE_LOOP('',(#1617));
#542=EDGE_LOOP('',(#1618,#1619,#1620,#1621));
#543=EDGE_LOOP('',(#1622,#1623,#1624,#1625));
#544=EDGE_LOOP('',(#1626,#1627,#1628,#1629));
#545=EDGE_LOOP('',(#1630,#1631,#1632,#1633));
#546=EDGE_LOOP('',(#1634));
#547=EDGE_LOOP('',(#1635));
#548=EDGE_LOOP('',(#1636));
#549=EDGE_LOOP('',(#1637));
#550=EDGE_LOOP('',(#1638));
#551=EDGE_LOOP('',(#1639));
#552=EDGE_LOOP('',(#1640));
#553=EDGE_LOOP('',(#1641));
#554=EDGE_LOOP('',(#1642));
#555=EDGE_LOOP('',(#1643));
#556=EDGE_LOOP('',(#1644));
#557=EDGE_LOOP('',(#1645));
#558=EDGE_LOOP('',(#1646,#1647,#1648,#1649,#1650,#1651));
#559=EDGE_LOOP('',(#1652,#1653,#1654,#1655,#1656));
#560=EDGE_LOOP('',(#1657,#1658,#1659,#1660));
#561=EDGE_LOOP('',(#1661,#1662,#1663,#1664));
#562=EDGE_LOOP('',(#1665));
#563=EDGE_LOOP('',(#1666));
#564=EDGE_LOOP('',(#1667,#1668,#1669,#1670,#1671));
#565=EDGE_LOOP('',(#1672));
#566=EDGE_LOOP('',(#1673));
#567=EDGE_LOOP('',(#1674,#1675,#1676,#1677));
#568=EDGE_LOOP('',(#1678,#1679,#1680,#1681,#1682,#1683));
#569=EDGE_LOOP('',(#1684,#1685,#1686,#1687,#1688));
#570=EDGE_LOOP('',(#1689));
#571=EDGE_LOOP('',(#1690));
#572=EDGE_LOOP('',(#1691,#1692,#1693,#1694));
#573=EDGE_LOOP('',(#1695,#1696,#1697,#1698));
#574=EDGE_LOOP('',(#1699,#1700,#1701,#1702));
#575=EDGE_LOOP('',(#1703));
#576=EDGE_LOOP('',(#1704));
#577=EDGE_LOOP('',(#1705,#1706,#1707,#1708,#1709));
#578=EDGE_LOOP('',(#1710,#1711));
#579=EDGE_LOOP('',(#1712,#1713));
#580=EDGE_LOOP('',(#1714,#1715));
#581=EDGE_LOOP('',(#1716,#1717));
#582=EDGE_LOOP('',(#1718,#1719));
#583=EDGE_LOOP('',(#1720,#1721));
#584=EDGE_LOOP('',(#1722,#1723));
#585=EDGE_LOOP('',(#1724,#1725));
#586=EDGE_LOOP('',(#1726,#1727,#1728,#1729));
#587=EDGE_LOOP('',(#1730,#1731,#1732,#1733,#1734,#1735,#1736,#1737,#1738,
#1739,#1740,#1741,#1742,#1743,#1744,#1745,#1746,#1747,#1748,#1749));
#588=EDGE_LOOP('',(#1750,#1751,#1752,#1753));
#589=EDGE_LOOP('',(#1754,#1755,#1756,#1757));
#590=EDGE_LOOP('',(#1758,#1759,#1760,#1761));
#591=EDGE_LOOP('',(#1762,#1763,#1764,#1765));
#592=EDGE_LOOP('',(#1766,#1767,#1768,#1769));
#593=EDGE_LOOP('',(#1770,#1771,#1772,#1773,#1774,#1775));
#594=EDGE_LOOP('',(#1776,#1777,#1778,#1779));
#595=EDGE_LOOP('',(#1780,#1781,#1782,#1783));
#596=EDGE_LOOP('',(#1784,#1785,#1786,#1787));
#597=EDGE_LOOP('',(#1788,#1789,#1790,#1791));
#598=EDGE_LOOP('',(#1792,#1793,#1794,#1795));
#599=EDGE_LOOP('',(#1796,#1797,#1798,#1799));
#600=EDGE_LOOP('',(#1800,#1801,#1802,#1803,#1804,#1805,#1806,#1807,#1808,
#1809,#1810,#1811,#1812,#1813,#1814,#1815,#1816,#1817,#1818,#1819));
#601=EDGE_LOOP('',(#1820,#1821,#1822,#1823));
#602=EDGE_LOOP('',(#1824,#1825,#1826,#1827));
#603=EDGE_LOOP('',(#1828));
#604=EDGE_LOOP('',(#1829));
#605=EDGE_LOOP('',(#1830,#1831,#1832,#1833));
#606=EDGE_LOOP('',(#1834));
#607=EDGE_LOOP('',(#1835));
#608=EDGE_LOOP('',(#1836,#1837,#1838,#1839));
#609=EDGE_LOOP('',(#1840));
#610=EDGE_LOOP('',(#1841));
#611=EDGE_LOOP('',(#1842,#1843,#1844,#1845));
#612=EDGE_LOOP('',(#1846));
#613=EDGE_LOOP('',(#1847));
#614=EDGE_LOOP('',(#1848,#1849,#1850,#1851));
#615=EDGE_LOOP('',(#1852));
#616=EDGE_LOOP('',(#1853));
#617=EDGE_LOOP('',(#1854,#1855,#1856,#1857));
#618=EDGE_LOOP('',(#1858,#1859,#1860,#1861));
#619=EDGE_LOOP('',(#1862,#1863,#1864,#1865));
#620=EDGE_LOOP('',(#1866));
#621=EDGE_LOOP('',(#1867));
#622=EDGE_LOOP('',(#1868));
#623=EDGE_LOOP('',(#1869));
#624=EDGE_LOOP('',(#1870,#1871,#1872,#1873));
#625=EDGE_LOOP('',(#1874,#1875,#1876,#1877));
#626=EDGE_LOOP('',(#1878,#1879,#1880,#1881));
#627=EDGE_LOOP('',(#1882,#1883,#1884,#1885));
#628=EDGE_LOOP('',(#1886,#1887,#1888,#1889));
#629=EDGE_LOOP('',(#1890));
#630=EDGE_LOOP('',(#1891));
#631=EDGE_LOOP('',(#1892,#1893,#1894,#1895));
#632=EDGE_LOOP('',(#1896));
#633=EDGE_LOOP('',(#1897));
#634=EDGE_LOOP('',(#1898,#1899,#1900,#1901));
#635=EDGE_LOOP('',(#1902,#1903,#1904,#1905));
#636=EDGE_LOOP('',(#1906));
#637=EDGE_LOOP('',(#1907));
#638=EDGE_LOOP('',(#1908));
#639=EDGE_LOOP('',(#1909));
#640=EDGE_LOOP('',(#1910));
#641=EDGE_LOOP('',(#1911));
#642=EDGE_LOOP('',(#1912));
#643=EDGE_LOOP('',(#1913));
#644=EDGE_LOOP('',(#1914));
#645=EDGE_LOOP('',(#1915));
#646=EDGE_LOOP('',(#1916));
#647=EDGE_LOOP('',(#1917));
#648=EDGE_LOOP('',(#1918,#1919,#1920,#1921));
#649=EDGE_LOOP('',(#1922,#1923,#1924,#1925));
#650=EDGE_LOOP('',(#1926));
#651=EDGE_LOOP('',(#1927));
#652=EDGE_LOOP('',(#1928));
#653=EDGE_LOOP('',(#1929));
#654=EDGE_LOOP('',(#1930,#1931,#1932,#1933));
#655=EDGE_LOOP('',(#1934,#1935,#1936,#1937));
#656=EDGE_LOOP('',(#1938,#1939,#1940,#1941));
#657=EDGE_LOOP('',(#1942,#1943,#1944,#1945));
#658=EDGE_LOOP('',(#1946,#1947,#1948,#1949));
#659=EDGE_LOOP('',(#1950));
#660=EDGE_LOOP('',(#1951));
#661=EDGE_LOOP('',(#1952,#1953,#1954,#1955));
#662=EDGE_LOOP('',(#1956,#1957,#1958,#1959));
#663=EDGE_LOOP('',(#1960));
#664=EDGE_LOOP('',(#1961));
#665=EDGE_LOOP('',(#1962));
#666=EDGE_LOOP('',(#1963));
#667=EDGE_LOOP('',(#1964));
#668=EDGE_LOOP('',(#1965));
#669=EDGE_LOOP('',(#1966));
#670=EDGE_LOOP('',(#1967));
#671=EDGE_LOOP('',(#1968));
#672=EDGE_LOOP('',(#1969));
#673=EDGE_LOOP('',(#1970));
#674=EDGE_LOOP('',(#1971));
#675=EDGE_LOOP('',(#1972));
#676=EDGE_LOOP('',(#1973,#1974,#1975,#1976));
#677=EDGE_LOOP('',(#1977,#1978,#1979,#1980));
#678=EDGE_LOOP('',(#1981,#1982,#1983,#1984));
#679=EDGE_LOOP('',(#1985));
#680=EDGE_LOOP('',(#1986));
#681=EDGE_LOOP('',(#1987,#1988,#1989,#1990));
#682=EDGE_LOOP('',(#1991,#1992,#1993,#1994));
#683=EDGE_LOOP('',(#1995,#1996,#1997,#1998));
#684=EDGE_LOOP('',(#1999));
#685=EDGE_LOOP('',(#2000,#2001,#2002,#2003));
#686=EDGE_LOOP('',(#2004,#2005,#2006,#2007));
#687=EDGE_LOOP('',(#2008,#2009,#2010,#2011));
#688=EDGE_LOOP('',(#2012,#2013,#2014,#2015));
#689=EDGE_LOOP('',(#2016,#2017,#2018,#2019));
#690=EDGE_LOOP('',(#2020,#2021,#2022,#2023));
#691=EDGE_LOOP('',(#2024,#2025,#2026,#2027,#2028,#2029));
#692=EDGE_LOOP('',(#2030,#2031,#2032,#2033,#2034,#2035));
#693=EDGE_LOOP('',(#2036,#2037,#2038,#2039));
#694=EDGE_LOOP('',(#2040));
#695=EDGE_LOOP('',(#2041));
#696=EDGE_LOOP('',(#2042));
#697=EDGE_LOOP('',(#2043));
#698=EDGE_LOOP('',(#2044,#2045,#2046,#2047));
#699=EDGE_LOOP('',(#2048));
#700=EDGE_LOOP('',(#2049));
#701=EDGE_LOOP('',(#2050));
#702=EDGE_LOOP('',(#2051));
#703=EDGE_LOOP('',(#2052,#2053,#2054,#2055));
#704=EDGE_LOOP('',(#2056,#2057,#2058,#2059));
#705=EDGE_LOOP('',(#2060,#2061,#2062,#2063));
#706=EDGE_LOOP('',(#2064));
#707=EDGE_LOOP('',(#2065));
#708=EDGE_LOOP('',(#2066,#2067,#2068,#2069));
#709=EDGE_LOOP('',(#2070,#2071,#2072,#2073));
#710=EDGE_LOOP('',(#2074));
#711=EDGE_LOOP('',(#2075));
#712=EDGE_LOOP('',(#2076));
#713=EDGE_LOOP('',(#2077));
#714=EDGE_LOOP('',(#2078,#2079,#2080,#2081));
#715=EDGE_LOOP('',(#2082,#2083,#2084,#2085));
#716=EDGE_LOOP('',(#2086,#2087,#2088,#2089));
#717=EDGE_LOOP('',(#2090));
#718=EDGE_LOOP('',(#2091));
#719=EDGE_LOOP('',(#2092,#2093,#2094,#2095));
#720=EDGE_LOOP('',(#2096,#2097,#2098,#2099));
#721=EDGE_LOOP('',(#2100,#2101,#2102,#2103));
#722=EDGE_LOOP('',(#2104,#2105,#2106,#2107));
#723=EDGE_LOOP('',(#2108,#2109,#2110,#2111));
#724=EDGE_LOOP('',(#2112));
#725=EDGE_LOOP('',(#2113));
#726=LINE('',#3690,#812);
#727=LINE('',#3696,#813);
#728=LINE('',#3702,#814);
#729=LINE('',#3708,#815);
#730=LINE('',#3714,#816);
#731=LINE('',#3721,#817);
#732=LINE('',#3728,#818);
#733=LINE('',#3735,#819);
#734=LINE('',#3742,#820);
#735=LINE('',#3749,#821);
#736=LINE('',#3756,#822);
#737=LINE('',#3763,#823);
#738=LINE('',#3777,#824);
#739=LINE('',#3780,#825);
#740=LINE('',#3786,#826);
#741=LINE('',#3791,#827);
#742=LINE('',#3808,#828);
#743=LINE('',#3814,#829);
#744=LINE('',#3818,#830);
#745=LINE('',#3824,#831);
#746=LINE('',#3829,#832);
#747=LINE('',#3844,#833);
#748=LINE('',#3853,#834);
#749=LINE('',#3857,#835);
#750=LINE('',#3861,#836);
#751=LINE('',#3864,#837);
#752=LINE('',#4017,#838);
#753=LINE('',#4313,#839);
#754=LINE('',#4355,#840);
#755=LINE('',#4360,#841);
#756=LINE('',#4369,#842);
#757=LINE('',#4374,#843);
#758=LINE('',#4385,#844);
#759=LINE('',#4391,#845);
#760=LINE('',#4400,#846);
#761=LINE('',#4406,#847);
#762=LINE('',#4412,#848);
#763=LINE('',#4418,#849);
#764=LINE('',#4424,#850);
#765=LINE('',#4433,#851);
#766=LINE('',#4439,#852);
#767=LINE('',#4444,#853);
#768=LINE('',#4453,#854);
#769=LINE('',#4459,#855);
#770=LINE('',#4468,#856);
#771=LINE('',#4474,#857);
#772=LINE('',#4480,#858);
#773=LINE('',#4486,#859);
#774=LINE('',#4492,#860);
#775=LINE('',#4500,#861);
#776=LINE('',#4505,#862);
#777=LINE('',#4516,#863);
#778=LINE('',#4520,#864);
#779=LINE('',#4524,#865);
#780=LINE('',#4531,#866);
#781=LINE('',#4535,#867);
#782=LINE('',#4539,#868);
#783=LINE('',#4544,#869);
#784=LINE('',#4546,#870);
#785=LINE('',#4548,#871);
#786=LINE('',#4549,#872);
#787=LINE('',#4552,#873);
#788=LINE('',#4554,#874);
#789=LINE('',#4555,#875);
#790=LINE('',#4558,#876);
#791=LINE('',#4560,#877);
#792=LINE('',#4561,#878);
#793=LINE('',#4564,#879);
#794=LINE('',#4566,#880);
#795=LINE('',#4567,#881);
#796=LINE('',#4570,#882);
#797=LINE('',#4572,#883);
#798=LINE('',#4573,#884);
#799=LINE('',#4575,#885);
#800=LINE('',#4576,#886);
#801=LINE('',#4600,#887);
#802=LINE('',#4610,#888);
#803=LINE('',#4621,#889);
#804=LINE('',#4624,#890);
#805=LINE('',#4629,#891);
#806=LINE('',#4637,#892);
#807=LINE('',#4643,#893);
#808=LINE('',#4651,#894);
#809=LINE('',#4655,#895);
#810=LINE('',#4872,#896);
#811=LINE('',#4876,#897);
#812=VECTOR('',#2877,0.44);
#813=VECTOR('',#2884,0.44);
#814=VECTOR('',#2891,0.44);
#815=VECTOR('',#2898,0.44);
#816=VECTOR('',#2905,0.165);
#817=VECTOR('',#2914,0.165);
#818=VECTOR('',#2923,0.165);
#819=VECTOR('',#2932,0.165);
#820=VECTOR('',#2941,0.165);
#821=VECTOR('',#2950,0.165);
#822=VECTOR('',#2959,0.165);
#823=VECTOR('',#2968,0.165);
#824=VECTOR('',#2987,5.);
#825=VECTOR('',#2990,3.5);
#826=VECTOR('',#2997,2.35);
#827=VECTOR('',#3004,3.5);
#828=VECTOR('',#3027,1.63531);
#829=VECTOR('',#3034,1.);
#830=VECTOR('',#3039,1.05);
#831=VECTOR('',#3048,1.63531);
#832=VECTOR('',#3055,1.05);
#833=VECTOR('',#3074,1.71469);
#834=VECTOR('',#3085,2.3);
#835=VECTOR('',#3090,2.35);
#836=VECTOR('',#3095,2.3);
#837=VECTOR('',#3100,1.71469);
#838=VECTOR('',#3151,1.706752);
#839=VECTOR('',#3228,1.643248);
#840=VECTOR('',#3257,1.70469);
#841=VECTOR('',#3264,1.65031);
#842=VECTOR('',#3275,1.70469);
#843=VECTOR('',#3282,1.65031);
#844=VECTOR('',#3299,1.75);
#845=VECTOR('',#3306,2.34);
#846=VECTOR('',#3319,0.225);
#847=VECTOR('',#3326,0.225);
#848=VECTOR('',#3333,0.225);
#849=VECTOR('',#3340,0.225);
#850=VECTOR('',#3347,2.34);
#851=VECTOR('',#3358,1.8);
#852=VECTOR('',#3367,1.6);
#853=VECTOR('',#3372,3.5);
#854=VECTOR('',#3385,1.);
#855=VECTOR('',#3392,1.8);
#856=VECTOR('',#3405,0.225);
#857=VECTOR('',#3412,0.225);
#858=VECTOR('',#3419,0.225);
#859=VECTOR('',#3426,0.225);
#860=VECTOR('',#3433,2.34);
#861=VECTOR('',#3444,1.8);
#862=VECTOR('',#3449,3.5);
#863=VECTOR('',#3466,0.325);
#864=VECTOR('',#3471,0.35);
#865=VECTOR('',#3476,0.335);
#866=VECTOR('',#3485,0.21);
#867=VECTOR('',#3490,0.2);
#868=VECTOR('',#3495,0.18);
#869=VECTOR('',#3500,1.);
#870=VECTOR('',#3501,1.);
#871=VECTOR('',#3502,1.);
#872=VECTOR('',#3503,1.);
#873=VECTOR('',#3506,1.);
#874=VECTOR('',#3507,1.);
#875=VECTOR('',#3508,1.);
#876=VECTOR('',#3511,1.);
#877=VECTOR('',#3512,1.);
#878=VECTOR('',#3513,1.);
#879=VECTOR('',#3516,1.);
#880=VECTOR('',#3517,1.);
#881=VECTOR('',#3518,1.);
#882=VECTOR('',#3521,1.);
#883=VECTOR('',#3522,1.);
#884=VECTOR('',#3523,1.);
#885=VECTOR('',#3526,1.);
#886=VECTOR('',#3527,1.);
#887=VECTOR('',#3570,0.95);
#888=VECTOR('',#3583,1.);
#889=VECTOR('',#3598,1.2);
#890=VECTOR('',#3601,1.);
#891=VECTOR('',#3608,1.);
#892=VECTOR('',#3619,1.01);
#893=VECTOR('',#3626,1.35);
#894=VECTOR('',#3637,1.);
#895=VECTOR('',#3640,1.);
#896=VECTOR('',#3659,0.1);
#897=VECTOR('',#3664,0.1);
#898=CIRCLE('',#2506,0.44);
#899=CIRCLE('',#2507,0.44);
#900=CIRCLE('',#2509,0.44);
#901=CIRCLE('',#2510,0.44);
#902=CIRCLE('',#2512,0.44);
#903=CIRCLE('',#2513,0.44);
#904=CIRCLE('',#2515,0.44);
#905=CIRCLE('',#2516,0.44);
#906=CIRCLE('',#2518,0.165);
#907=CIRCLE('',#2519,0.165);
#908=CIRCLE('',#2522,0.165);
#909=CIRCLE('',#2523,0.165);
#910=CIRCLE('',#2526,0.165);
#911=CIRCLE('',#2527,0.165);
#912=CIRCLE('',#2530,0.165);
#913=CIRCLE('',#2531,0.165);
#914=CIRCLE('',#2534,0.165);
#915=CIRCLE('',#2535,0.165);
#916=CIRCLE('',#2538,0.165);
#917=CIRCLE('',#2539,0.165);
#918=CIRCLE('',#2542,0.165);
#919=CIRCLE('',#2543,0.165);
#920=CIRCLE('',#2546,0.165);
#921=CIRCLE('',#2547,0.165);
#922=CIRCLE('',#2550,5.);
#923=CIRCLE('',#2551,3.5);
#924=CIRCLE('',#2553,5.);
#925=CIRCLE('',#2554,3.5);
#926=CIRCLE('',#2557,3.5);
#927=CIRCLE('',#2559,2.35);
#928=CIRCLE('',#2560,2.35);
#929=CIRCLE('',#2562,3.5);
#930=CIRCLE('',#2568,1.63531);
#931=CIRCLE('',#2569,1.63531);
#932=CIRCLE('',#2570,0.412776);
#933=CIRCLE('',#2571,1.63531);
#934=CIRCLE('',#2572,1.63531);
#935=CIRCLE('',#2574,1.63531);
#936=CIRCLE('',#2576,1.);
#937=CIRCLE('',#2577,1.);
#938=CIRCLE('',#2579,1.1);
#939=CIRCLE('',#2582,1.63531);
#940=CIRCLE('',#2584,1.1);
#941=CIRCLE('',#2588,1.71469);
#942=CIRCLE('',#2589,1.71469);
#943=CIRCLE('',#2590,0.412776);
#944=CIRCLE('',#2591,1.71469);
#945=CIRCLE('',#2592,1.71469);
#946=CIRCLE('',#2594,1.71469);
#947=CIRCLE('',#2596,2.25);
#948=CIRCLE('',#2597,1.71469);
#949=CIRCLE('',#2599,2.35);
#950=CIRCLE('',#2601,2.35);
#951=CIRCLE('',#2603,2.25);
#952=CIRCLE('',#2608,0.3969);
#953=CIRCLE('',#2610,0.3969);
#954=CIRCLE('',#2612,0.3969);
#955=CIRCLE('',#2614,0.3969);
#956=CIRCLE('',#2616,0.3969);
#957=CIRCLE('',#2618,0.3969);
#958=CIRCLE('',#2620,0.3969);
#959=CIRCLE('',#2622,0.3969);
#960=CIRCLE('',#2625,0.405071403305639);
#961=CIRCLE('',#2626,0.405071403305639);
#962=CIRCLE('',#2628,1.706752);
#963=CIRCLE('',#2629,1.706752);
#964=CIRCLE('',#2630,1.706752);
#965=CIRCLE('',#2631,1.706752);
#966=CIRCLE('',#2632,1.706752);
#967=CIRCLE('',#2633,1.706752);
#968=CIRCLE('',#2634,1.706752);
#969=CIRCLE('',#2635,1.706752);
#970=CIRCLE('',#2636,1.706752);
#971=CIRCLE('',#2638,1.643248);
#972=CIRCLE('',#2639,0.405071403305639);
#973=CIRCLE('',#2641,0.405071403305639);
#974=CIRCLE('',#2643,1.643248);
#975=CIRCLE('',#2644,0.405071403305639);
#976=CIRCLE('',#2646,0.405071403305639);
#977=CIRCLE('',#2648,1.643248);
#978=CIRCLE('',#2649,0.405071403305639);
#979=CIRCLE('',#2651,0.405071403305639);
#980=CIRCLE('',#2653,1.643248);
#981=CIRCLE('',#2654,0.405071403305639);
#982=CIRCLE('',#2656,0.405071403305639);
#983=CIRCLE('',#2658,1.643248);
#984=CIRCLE('',#2659,0.405071403305639);
#985=CIRCLE('',#2661,0.405071403305639);
#986=CIRCLE('',#2663,1.643248);
#987=CIRCLE('',#2664,0.405071403305639);
#988=CIRCLE('',#2666,0.405071403305639);
#989=CIRCLE('',#2668,1.643248);
#990=CIRCLE('',#2669,1.643248);
#991=CIRCLE('',#2670,1.643248);
#992=CIRCLE('',#2672,0.405071403305639);
#993=CIRCLE('',#2674,0.405071403305639);
#994=CIRCLE('',#2679,1.70469);
#995=CIRCLE('',#2680,1.65031);
#996=CIRCLE('',#2682,1.70469);
#997=CIRCLE('',#2684,1.65031);
#998=CIRCLE('',#2687,1.70469);
#999=CIRCLE('',#2688,1.65031);
#1000=CIRCLE('',#2690,1.70469);
#1001=CIRCLE('',#2692,1.65031);
#1002=CIRCLE('',#2701,1.75);
#1003=CIRCLE('',#2702,1.75);
#1004=CIRCLE('',#2704,2.34);
#1005=CIRCLE('',#2705,2.34);
#1006=CIRCLE('',#2710,0.225);
#1007=CIRCLE('',#2711,0.225);
#1008=CIRCLE('',#2713,0.225);
#1009=CIRCLE('',#2714,0.225);
#1010=CIRCLE('',#2716,0.225);
#1011=CIRCLE('',#2717,0.225);
#1012=CIRCLE('',#2719,0.225);
#1013=CIRCLE('',#2720,0.225);
#1014=CIRCLE('',#2722,2.34);
#1015=CIRCLE('',#2723,2.34);
#1016=CIRCLE('',#2725,1.6);
#1017=CIRCLE('',#2727,1.8);
#1018=CIRCLE('',#2728,1.8);
#1019=CIRCLE('',#2730,1.6);
#1020=CIRCLE('',#2733,3.5);
#1021=CIRCLE('',#2734,3.5);
#1022=CIRCLE('',#2739,1.);
#1023=CIRCLE('',#2740,1.);
#1024=CIRCLE('',#2742,1.8);
#1025=CIRCLE('',#2743,1.8);
#1026=CIRCLE('',#2748,0.225);
#1027=CIRCLE('',#2749,0.225);
#1028=CIRCLE('',#2751,0.225);
#1029=CIRCLE('',#2752,0.225);
#1030=CIRCLE('',#2754,0.225);
#1031=CIRCLE('',#2755,0.225);
#1032=CIRCLE('',#2757,0.225);
#1033=CIRCLE('',#2758,0.225);
#1034=CIRCLE('',#2760,2.34);
#1035=CIRCLE('',#2761,2.34);
#1036=CIRCLE('',#2763,1.8);
#1037=CIRCLE('',#2765,1.8);
#1038=CIRCLE('',#2767,3.5);
#1039=CIRCLE('',#2768,3.5);
#1040=CIRCLE('',#2773,0.3);
#1041=CIRCLE('',#2775,0.35);
#1042=CIRCLE('',#2777,0.35);
#1043=CIRCLE('',#2779,0.32);
#1044=CIRCLE('',#2781,0.22);
#1045=CIRCLE('',#2783,0.1954);
#1046=CIRCLE('',#2785,0.1954);
#1047=CIRCLE('',#2787,0.16);
#1048=CIRCLE('',#2815,0.95);
#1049=CIRCLE('',#2816,0.95);
#1050=CIRCLE('',#2818,1.);
#1051=CIRCLE('',#2820,1.);
#1052=CIRCLE('',#2822,1.);
#1053=CIRCLE('',#2824,1.2);
#1054=CIRCLE('',#2826,1.2);
#1055=CIRCLE('',#2827,1.);
#1056=CIRCLE('',#2830,1.);
#1057=CIRCLE('',#2832,1.);
#1058=CIRCLE('',#2837,1.01);
#1059=CIRCLE('',#2838,1.01);
#1060=CIRCLE('',#2840,1.35);
#1061=CIRCLE('',#2841,1.35);
#1062=CIRCLE('',#2846,0.95);
#1063=CIRCLE('',#2847,0.95);
#1064=CIRCLE('',#2849,0.1612);
#1065=CIRCLE('',#2850,0.1612);
#1066=CIRCLE('',#2852,0.1612);
#1067=CIRCLE('',#2853,0.1);
#1068=CIRCLE('',#2854,0.1);
#1069=CIRCLE('',#2856,0.1);
#1070=CIRCLE('',#2858,0.1);
#1071=CIRCLE('',#2860,0.1612);
#1072=VERTEX_POINT('',#3687);
#1073=VERTEX_POINT('',#3689);
#1074=VERTEX_POINT('',#3693);
#1075=VERTEX_POINT('',#3695);
#1076=VERTEX_POINT('',#3699);
#1077=VERTEX_POINT('',#3701);
#1078=VERTEX_POINT('',#3705);
#1079=VERTEX_POINT('',#3707);
#1080=VERTEX_POINT('',#3711);
#1081=VERTEX_POINT('',#3713);
#1082=VERTEX_POINT('',#3718);
#1083=VERTEX_POINT('',#3720);
#1084=VERTEX_POINT('',#3725);
#1085=VERTEX_POINT('',#3727);
#1086=VERTEX_POINT('',#3732);
#1087=VERTEX_POINT('',#3734);
#1088=VERTEX_POINT('',#3739);
#1089=VERTEX_POINT('',#3741);
#1090=VERTEX_POINT('',#3746);
#1091=VERTEX_POINT('',#3748);
#1092=VERTEX_POINT('',#3753);
#1093=VERTEX_POINT('',#3755);
#1094=VERTEX_POINT('',#3760);
#1095=VERTEX_POINT('',#3762);
#1096=VERTEX_POINT('',#3767);
#1097=VERTEX_POINT('',#3769);
#1098=VERTEX_POINT('',#3772);
#1099=VERTEX_POINT('',#3774);
#1100=VERTEX_POINT('',#3779);
#1101=VERTEX_POINT('',#3783);
#1102=VERTEX_POINT('',#3785);
#1103=VERTEX_POINT('',#3789);
#1104=VERTEX_POINT('',#3797);
#1105=VERTEX_POINT('',#3798);
#1106=VERTEX_POINT('',#3801);
#1107=VERTEX_POINT('',#3803);
#1108=VERTEX_POINT('',#3807);
#1109=VERTEX_POINT('',#3811);
#1110=VERTEX_POINT('',#3813);
#1111=VERTEX_POINT('',#3817);
#1112=VERTEX_POINT('',#3822);
#1113=VERTEX_POINT('',#3826);
#1114=VERTEX_POINT('',#3832);
#1115=VERTEX_POINT('',#3833);
#1116=VERTEX_POINT('',#3836);
#1117=VERTEX_POINT('',#3838);
#1118=VERTEX_POINT('',#3842);
#1119=VERTEX_POINT('',#3846);
#1120=VERTEX_POINT('',#3848);
#1121=VERTEX_POINT('',#3851);
#1122=VERTEX_POINT('',#3855);
#1123=VERTEX_POINT('',#3859);
#1124=VERTEX_POINT('',#3867);
#1125=VERTEX_POINT('',#3868);
#1126=VERTEX_POINT('',#3871);
#1127=VERTEX_POINT('',#3872);
#1128=VERTEX_POINT('',#3875);
#1129=VERTEX_POINT('',#3876);
#1130=VERTEX_POINT('',#3879);
#1131=VERTEX_POINT('',#3880);
#1132=VERTEX_POINT('',#3883);
#1133=VERTEX_POINT('',#3884);
#1134=VERTEX_POINT('',#3887);
#1135=VERTEX_POINT('',#3888);
#1136=VERTEX_POINT('',#3891);
#1137=VERTEX_POINT('',#3892);
#1138=VERTEX_POINT('',#3895);
#1139=VERTEX_POINT('',#3896);
#1140=VERTEX_POINT('',#3900);
#1141=VERTEX_POINT('',#3901);
#1142=VERTEX_POINT('',#3924);
#1143=VERTEX_POINT('',#3926);
#1144=VERTEX_POINT('',#3951);
#1145=VERTEX_POINT('',#3953);
#1146=VERTEX_POINT('',#3976);
#1147=VERTEX_POINT('',#3978);
#1148=VERTEX_POINT('',#4001);
#1149=VERTEX_POINT('',#4003);
#1150=VERTEX_POINT('',#4016);
#1151=VERTEX_POINT('',#4019);
#1152=VERTEX_POINT('',#4032);
#1153=VERTEX_POINT('',#4034);
#1154=VERTEX_POINT('',#4057);
#1155=VERTEX_POINT('',#4059);
#1156=VERTEX_POINT('',#4082);
#1157=VERTEX_POINT('',#4084);
#1158=VERTEX_POINT('',#4107);
#1159=VERTEX_POINT('',#4109);
#1160=VERTEX_POINT('',#4134);
#1161=VERTEX_POINT('',#4138);
#1162=VERTEX_POINT('',#4163);
#1163=VERTEX_POINT('',#4167);
#1164=VERTEX_POINT('',#4192);
#1165=VERTEX_POINT('',#4196);
#1166=VERTEX_POINT('',#4197);
#1167=VERTEX_POINT('',#4224);
#1168=VERTEX_POINT('',#4228);
#1169=VERTEX_POINT('',#4253);
#1170=VERTEX_POINT('',#4257);
#1171=VERTEX_POINT('',#4282);
#1172=VERTEX_POINT('',#4286);
#1173=VERTEX_POINT('',#4311);
#1174=VERTEX_POINT('',#4314);
#1175=VERTEX_POINT('',#4316);
#1176=VERTEX_POINT('',#4348);
#1177=VERTEX_POINT('',#4350);
#1178=VERTEX_POINT('',#4353);
#1179=VERTEX_POINT('',#4357);
#1180=VERTEX_POINT('',#4362);
#1181=VERTEX_POINT('',#4364);
#1182=VERTEX_POINT('',#4367);
#1183=VERTEX_POINT('',#4371);
#1184=VERTEX_POINT('',#4382);
#1185=VERTEX_POINT('',#4384);
#1186=VERTEX_POINT('',#4388);
#1187=VERTEX_POINT('',#4390);
#1188=VERTEX_POINT('',#4397);
#1189=VERTEX_POINT('',#4399);
#1190=VERTEX_POINT('',#4403);
#1191=VERTEX_POINT('',#4405);
#1192=VERTEX_POINT('',#4409);
#1193=VERTEX_POINT('',#4411);
#1194=VERTEX_POINT('',#4415);
#1195=VERTEX_POINT('',#4417);
#1196=VERTEX_POINT('',#4421);
#1197=VERTEX_POINT('',#4423);
#1198=VERTEX_POINT('',#4427);
#1199=VERTEX_POINT('',#4430);
#1200=VERTEX_POINT('',#4432);
#1201=VERTEX_POINT('',#4436);
#1202=VERTEX_POINT('',#4441);
#1203=VERTEX_POINT('',#4443);
#1204=VERTEX_POINT('',#4450);
#1205=VERTEX_POINT('',#4452);
#1206=VERTEX_POINT('',#4456);
#1207=VERTEX_POINT('',#4458);
#1208=VERTEX_POINT('',#4465);
#1209=VERTEX_POINT('',#4467);
#1210=VERTEX_POINT('',#4471);
#1211=VERTEX_POINT('',#4473);
#1212=VERTEX_POINT('',#4477);
#1213=VERTEX_POINT('',#4479);
#1214=VERTEX_POINT('',#4483);
#1215=VERTEX_POINT('',#4485);
#1216=VERTEX_POINT('',#4489);
#1217=VERTEX_POINT('',#4491);
#1218=VERTEX_POINT('',#4495);
#1219=VERTEX_POINT('',#4498);
#1220=VERTEX_POINT('',#4502);
#1221=VERTEX_POINT('',#4504);
#1222=VERTEX_POINT('',#4511);
#1223=VERTEX_POINT('',#4514);
#1224=VERTEX_POINT('',#4518);
#1225=VERTEX_POINT('',#4522);
#1226=VERTEX_POINT('',#4526);
#1227=VERTEX_POINT('',#4529);
#1228=VERTEX_POINT('',#4533);
#1229=VERTEX_POINT('',#4537);
#1230=VERTEX_POINT('',#4542);
#1231=VERTEX_POINT('',#4543);
#1232=VERTEX_POINT('',#4545);
#1233=VERTEX_POINT('',#4547);
#1234=VERTEX_POINT('',#4551);
#1235=VERTEX_POINT('',#4553);
#1236=VERTEX_POINT('',#4557);
#1237=VERTEX_POINT('',#4559);
#1238=VERTEX_POINT('',#4563);
#1239=VERTEX_POINT('',#4565);
#1240=VERTEX_POINT('',#4569);
#1241=VERTEX_POINT('',#4571);
#1242=VERTEX_POINT('',#4597);
#1243=VERTEX_POINT('',#4599);
#1244=VERTEX_POINT('',#4603);
#1245=VERTEX_POINT('',#4606);
#1246=VERTEX_POINT('',#4609);
#1247=VERTEX_POINT('',#4613);
#1248=VERTEX_POINT('',#4616);
#1249=VERTEX_POINT('',#4618);
#1250=VERTEX_POINT('',#4623);
#1251=VERTEX_POINT('',#4627);
#1252=VERTEX_POINT('',#4634);
#1253=VERTEX_POINT('',#4636);
#1254=VERTEX_POINT('',#4640);
#1255=VERTEX_POINT('',#4642);
#1256=VERTEX_POINT('',#4649);
#1257=VERTEX_POINT('',#4650);
#1258=VERTEX_POINT('',#4652);
#1259=VERTEX_POINT('',#4654);
#1260=VERTEX_POINT('',#4658);
#1261=VERTEX_POINT('',#4660);
#1262=VERTEX_POINT('',#4669);
#1263=VERTEX_POINT('',#4866);
#1264=VERTEX_POINT('',#4868);
#1265=VERTEX_POINT('',#4871);
#1266=VERTEX_POINT('',#4875);
#1267=VERTEX_POINT('',#4879);
#1268=EDGE_CURVE('',#1072,#1072,#898,.T.);
#1269=EDGE_CURVE('',#1072,#1073,#726,.T.);
#1270=EDGE_CURVE('',#1073,#1073,#899,.T.);
#1271=EDGE_CURVE('',#1074,#1074,#900,.T.);
#1272=EDGE_CURVE('',#1074,#1075,#727,.T.);
#1273=EDGE_CURVE('',#1075,#1075,#901,.T.);
#1274=EDGE_CURVE('',#1076,#1076,#902,.T.);
#1275=EDGE_CURVE('',#1076,#1077,#728,.T.);
#1276=EDGE_CURVE('',#1077,#1077,#903,.T.);
#1277=EDGE_CURVE('',#1078,#1078,#904,.T.);
#1278=EDGE_CURVE('',#1078,#1079,#729,.T.);
#1279=EDGE_CURVE('',#1079,#1079,#905,.T.);
#1280=EDGE_CURVE('',#1080,#1080,#906,.T.);
#1281=EDGE_CURVE('',#1080,#1081,#730,.T.);
#1282=EDGE_CURVE('',#1081,#1081,#907,.T.);
#1283=EDGE_CURVE('',#1082,#1082,#908,.T.);
#1284=EDGE_CURVE('',#1082,#1083,#731,.T.);
#1285=EDGE_CURVE('',#1083,#1083,#909,.T.);
#1286=EDGE_CURVE('',#1084,#1084,#910,.T.);
#1287=EDGE_CURVE('',#1084,#1085,#732,.T.);
#1288=EDGE_CURVE('',#1085,#1085,#911,.T.);
#1289=EDGE_CURVE('',#1086,#1086,#912,.T.);
#1290=EDGE_CURVE('',#1086,#1087,#733,.T.);
#1291=EDGE_CURVE('',#1087,#1087,#913,.T.);
#1292=EDGE_CURVE('',#1088,#1088,#914,.T.);
#1293=EDGE_CURVE('',#1088,#1089,#734,.T.);
#1294=EDGE_CURVE('',#1089,#1089,#915,.T.);
#1295=EDGE_CURVE('',#1090,#1090,#916,.T.);
#1296=EDGE_CURVE('',#1090,#1091,#735,.T.);
#1297=EDGE_CURVE('',#1091,#1091,#917,.T.);
#1298=EDGE_CURVE('',#1092,#1092,#918,.T.);
#1299=EDGE_CURVE('',#1092,#1093,#736,.T.);
#1300=EDGE_CURVE('',#1093,#1093,#919,.T.);
#1301=EDGE_CURVE('',#1094,#1094,#920,.T.);
#1302=EDGE_CURVE('',#1094,#1095,#737,.T.);
#1303=EDGE_CURVE('',#1095,#1095,#921,.T.);
#1304=EDGE_CURVE('',#1096,#1096,#922,.T.);
#1305=EDGE_CURVE('',#1097,#1097,#923,.T.);
#1306=EDGE_CURVE('',#1098,#1098,#924,.T.);
#1307=EDGE_CURVE('',#1099,#1099,#925,.T.);
#1308=EDGE_CURVE('',#1096,#1098,#738,.T.);
#1309=EDGE_CURVE('',#1099,#1100,#739,.T.);
#1310=EDGE_CURVE('',#1100,#1100,#926,.T.);
#1311=EDGE_CURVE('',#1101,#1101,#927,.T.);
#1312=EDGE_CURVE('',#1101,#1102,#740,.T.);
#1313=EDGE_CURVE('',#1102,#1102,#928,.T.);
#1314=EDGE_CURVE('',#1103,#1103,#929,.T.);
#1315=EDGE_CURVE('',#1103,#1097,#741,.T.);
#1316=EDGE_CURVE('',#1104,#1105,#930,.T.);
#1317=EDGE_CURVE('',#1105,#1104,#931,.T.);
#1318=EDGE_CURVE('',#1105,#1106,#932,.T.);
#1319=EDGE_CURVE('',#1107,#1106,#933,.T.);
#1320=EDGE_CURVE('',#1106,#1107,#934,.T.);
#1321=EDGE_CURVE('',#1107,#1108,#742,.T.);
#1322=EDGE_CURVE('',#1108,#1108,#935,.T.);
#1323=EDGE_CURVE('',#1109,#1109,#936,.T.);
#1324=EDGE_CURVE('',#1109,#1110,#743,.T.);
#1325=EDGE_CURVE('',#1110,#1110,#937,.T.);
#1326=EDGE_CURVE('',#1110,#1111,#744,.T.);
#1327=EDGE_CURVE('',#1111,#1111,#938,.T.);
#1328=EDGE_CURVE('',#1112,#1112,#939,.T.);
#1329=EDGE_CURVE('',#1112,#1104,#745,.T.);
#1330=EDGE_CURVE('',#1113,#1113,#940,.T.);
#1331=EDGE_CURVE('',#1113,#1109,#746,.T.);
#1332=EDGE_CURVE('',#1114,#1115,#941,.T.);
#1333=EDGE_CURVE('',#1115,#1114,#942,.T.);
#1334=EDGE_CURVE('',#1115,#1116,#943,.T.);
#1335=EDGE_CURVE('',#1117,#1116,#944,.T.);
#1336=EDGE_CURVE('',#1116,#1117,#945,.T.);
#1337=EDGE_CURVE('',#1118,#1118,#946,.T.);
#1338=EDGE_CURVE('',#1118,#1117,#747,.T.);
#1339=EDGE_CURVE('',#1119,#1119,#947,.T.);
#1340=EDGE_CURVE('',#1120,#1120,#948,.T.);
#1341=EDGE_CURVE('',#1121,#1121,#949,.T.);
#1342=EDGE_CURVE('',#1121,#1119,#748,.T.);
#1343=EDGE_CURVE('',#1122,#1122,#950,.T.);
#1344=EDGE_CURVE('',#1122,#1121,#749,.T.);
#1345=EDGE_CURVE('',#1123,#1123,#951,.T.);
#1346=EDGE_CURVE('',#1123,#1122,#750,.T.);
#1347=EDGE_CURVE('',#1114,#1120,#751,.T.);
#1348=EDGE_CURVE('',#1124,#1125,#952,.T.);
#1349=EDGE_CURVE('',#1126,#1127,#953,.T.);
#1350=EDGE_CURVE('',#1128,#1129,#954,.T.);
#1351=EDGE_CURVE('',#1130,#1131,#955,.T.);
#1352=EDGE_CURVE('',#1132,#1133,#956,.T.);
#1353=EDGE_CURVE('',#1134,#1135,#957,.T.);
#1354=EDGE_CURVE('',#1136,#1137,#958,.T.);
#1355=EDGE_CURVE('',#1138,#1139,#959,.T.);
#1356=EDGE_CURVE('',#1140,#1141,#116,.T.);
#1357=EDGE_CURVE('',#1142,#1140,#960,.T.);
#1358=EDGE_CURVE('',#1143,#1142,#117,.T.);
#1359=EDGE_CURVE('',#1141,#1143,#961,.T.);
#1360=EDGE_CURVE('',#1144,#1142,#962,.T.);
#1361=EDGE_CURVE('',#1144,#1145,#118,.T.);
#1362=EDGE_CURVE('',#1146,#1145,#963,.T.);
#1363=EDGE_CURVE('',#1146,#1147,#119,.T.);
#1364=EDGE_CURVE('',#1148,#1147,#964,.T.);
#1365=EDGE_CURVE('',#1148,#1149,#120,.T.);
#1366=EDGE_CURVE('',#1149,#1150,#752,.T.);
#1367=EDGE_CURVE('',#1150,#1150,#965,.T.);
#1368=EDGE_CURVE('',#1149,#1151,#121,.T.);
#1369=EDGE_CURVE('',#1152,#1151,#966,.T.);
#1370=EDGE_CURVE('',#1152,#1153,#122,.T.);
#1371=EDGE_CURVE('',#1154,#1153,#967,.T.);
#1372=EDGE_CURVE('',#1154,#1155,#123,.T.);
#1373=EDGE_CURVE('',#1156,#1155,#968,.T.);
#1374=EDGE_CURVE('',#1156,#1157,#124,.T.);
#1375=EDGE_CURVE('',#1158,#1157,#969,.T.);
#1376=EDGE_CURVE('',#1158,#1159,#125,.T.);
#1377=EDGE_CURVE('',#1143,#1159,#970,.T.);
#1378=EDGE_CURVE('',#1140,#1160,#971,.T.);
#1379=EDGE_CURVE('',#1160,#1144,#972,.T.);
#1380=EDGE_CURVE('',#1161,#1160,#126,.T.);
#1381=EDGE_CURVE('',#1145,#1161,#973,.T.);
#1382=EDGE_CURVE('',#1161,#1162,#974,.T.);
#1383=EDGE_CURVE('',#1162,#1146,#975,.T.);
#1384=EDGE_CURVE('',#1163,#1162,#127,.T.);
#1385=EDGE_CURVE('',#1147,#1163,#976,.T.);
#1386=EDGE_CURVE('',#1163,#1164,#977,.T.);
#1387=EDGE_CURVE('',#1164,#1148,#978,.T.);
#1388=EDGE_CURVE('',#1165,#1166,#128,.T.);
#1389=EDGE_CURVE('',#1151,#1165,#979,.T.);
#1390=EDGE_CURVE('',#1166,#1164,#129,.T.);
#1391=EDGE_CURVE('',#1165,#1167,#980,.T.);
#1392=EDGE_CURVE('',#1167,#1152,#981,.T.);
#1393=EDGE_CURVE('',#1168,#1167,#130,.T.);
#1394=EDGE_CURVE('',#1153,#1168,#982,.T.);
#1395=EDGE_CURVE('',#1168,#1169,#983,.T.);
#1396=EDGE_CURVE('',#1169,#1154,#984,.T.);
#1397=EDGE_CURVE('',#1170,#1169,#131,.T.);
#1398=EDGE_CURVE('',#1155,#1170,#985,.T.);
#1399=EDGE_CURVE('',#1170,#1171,#986,.T.);
#1400=EDGE_CURVE('',#1171,#1156,#987,.T.);
#1401=EDGE_CURVE('',#1172,#1171,#132,.T.);
#1402=EDGE_CURVE('',#1157,#1172,#988,.T.);
#1403=EDGE_CURVE('',#1173,#1173,#989,.T.);
#1404=EDGE_CURVE('',#1173,#1166,#753,.T.);
#1405=EDGE_CURVE('',#1174,#1141,#990,.T.);
#1406=EDGE_CURVE('',#1174,#1175,#133,.T.);
#1407=EDGE_CURVE('',#1172,#1175,#991,.T.);
#1408=EDGE_CURVE('',#1159,#1174,#992,.T.);
#1409=EDGE_CURVE('',#1175,#1158,#993,.T.);
#1410=EDGE_CURVE('',#1176,#1176,#994,.T.);
#1411=EDGE_CURVE('',#1177,#1177,#995,.T.);
#1412=EDGE_CURVE('',#1178,#1178,#996,.T.);
#1413=EDGE_CURVE('',#1178,#1176,#754,.T.);
#1414=EDGE_CURVE('',#1179,#1179,#997,.T.);
#1415=EDGE_CURVE('',#1179,#1177,#755,.T.);
#1416=EDGE_CURVE('',#1180,#1180,#998,.T.);
#1417=EDGE_CURVE('',#1181,#1181,#999,.T.);
#1418=EDGE_CURVE('',#1182,#1182,#1000,.T.);
#1419=EDGE_CURVE('',#1182,#1180,#756,.T.);
#1420=EDGE_CURVE('',#1183,#1183,#1001,.T.);
#1421=EDGE_CURVE('',#1183,#1181,#757,.T.);
#1422=EDGE_CURVE('',#1184,#1184,#1002,.T.);
#1423=EDGE_CURVE('',#1184,#1185,#758,.T.);
#1424=EDGE_CURVE('',#1185,#1185,#1003,.T.);
#1425=EDGE_CURVE('',#1186,#1186,#1004,.T.);
#1426=EDGE_CURVE('',#1186,#1187,#759,.T.);
#1427=EDGE_CURVE('',#1187,#1187,#1005,.T.);
#1428=EDGE_CURVE('',#1188,#1188,#1006,.T.);
#1429=EDGE_CURVE('',#1188,#1189,#760,.T.);
#1430=EDGE_CURVE('',#1189,#1189,#1007,.T.);
#1431=EDGE_CURVE('',#1190,#1190,#1008,.T.);
#1432=EDGE_CURVE('',#1190,#1191,#761,.T.);
#1433=EDGE_CURVE('',#1191,#1191,#1009,.T.);
#1434=EDGE_CURVE('',#1192,#1192,#1010,.T.);
#1435=EDGE_CURVE('',#1192,#1193,#762,.T.);
#1436=EDGE_CURVE('',#1193,#1193,#1011,.T.);
#1437=EDGE_CURVE('',#1194,#1194,#1012,.T.);
#1438=EDGE_CURVE('',#1194,#1195,#763,.T.);
#1439=EDGE_CURVE('',#1195,#1195,#1013,.T.);
#1440=EDGE_CURVE('',#1196,#1196,#1014,.T.);
#1441=EDGE_CURVE('',#1196,#1197,#764,.T.);
#1442=EDGE_CURVE('',#1197,#1197,#1015,.T.);
#1443=EDGE_CURVE('',#1198,#1198,#1016,.T.);
#1444=EDGE_CURVE('',#1199,#1199,#1017,.T.);
#1445=EDGE_CURVE('',#1199,#1200,#765,.T.);
#1446=EDGE_CURVE('',#1200,#1200,#1018,.T.);
#1447=EDGE_CURVE('',#1201,#1201,#1019,.T.);
#1448=EDGE_CURVE('',#1198,#1201,#766,.T.);
#1449=EDGE_CURVE('',#1202,#1202,#1020,.T.);
#1450=EDGE_CURVE('',#1202,#1203,#767,.T.);
#1451=EDGE_CURVE('',#1203,#1203,#1021,.T.);
#1452=EDGE_CURVE('',#1204,#1204,#1022,.T.);
#1453=EDGE_CURVE('',#1204,#1205,#768,.T.);
#1454=EDGE_CURVE('',#1205,#1205,#1023,.T.);
#1455=EDGE_CURVE('',#1206,#1206,#1024,.T.);
#1456=EDGE_CURVE('',#1206,#1207,#769,.T.);
#1457=EDGE_CURVE('',#1207,#1207,#1025,.T.);
#1458=EDGE_CURVE('',#1208,#1208,#1026,.T.);
#1459=EDGE_CURVE('',#1208,#1209,#770,.T.);
#1460=EDGE_CURVE('',#1209,#1209,#1027,.T.);
#1461=EDGE_CURVE('',#1210,#1210,#1028,.T.);
#1462=EDGE_CURVE('',#1210,#1211,#771,.T.);
#1463=EDGE_CURVE('',#1211,#1211,#1029,.T.);
#1464=EDGE_CURVE('',#1212,#1212,#1030,.T.);
#1465=EDGE_CURVE('',#1212,#1213,#772,.T.);
#1466=EDGE_CURVE('',#1213,#1213,#1031,.T.);
#1467=EDGE_CURVE('',#1214,#1214,#1032,.T.);
#1468=EDGE_CURVE('',#1214,#1215,#773,.T.);
#1469=EDGE_CURVE('',#1215,#1215,#1033,.T.);
#1470=EDGE_CURVE('',#1216,#1216,#1034,.T.);
#1471=EDGE_CURVE('',#1216,#1217,#774,.T.);
#1472=EDGE_CURVE('',#1217,#1217,#1035,.T.);
#1473=EDGE_CURVE('',#1218,#1218,#1036,.T.);
#1474=EDGE_CURVE('',#1219,#1219,#1037,.T.);
#1475=EDGE_CURVE('',#1219,#1218,#775,.T.);
#1476=EDGE_CURVE('',#1220,#1220,#1038,.T.);
#1477=EDGE_CURVE('',#1220,#1221,#776,.T.);
#1478=EDGE_CURVE('',#1221,#1221,#1039,.T.);
#1479=EDGE_CURVE('',#1222,#1222,#1040,.T.);
#1480=EDGE_CURVE('',#1223,#1223,#1041,.T.);
#1481=EDGE_CURVE('',#1223,#1222,#777,.T.);
#1482=EDGE_CURVE('',#1224,#1224,#1042,.T.);
#1483=EDGE_CURVE('',#1224,#1223,#778,.T.);
#1484=EDGE_CURVE('',#1225,#1225,#1043,.T.);
#1485=EDGE_CURVE('',#1225,#1224,#779,.T.);
#1486=EDGE_CURVE('',#1226,#1226,#1044,.T.);
#1487=EDGE_CURVE('',#1227,#1227,#1045,.F.);
#1488=EDGE_CURVE('',#1227,#1226,#780,.T.);
#1489=EDGE_CURVE('',#1228,#1228,#1046,.F.);
#1490=EDGE_CURVE('',#1228,#1227,#781,.T.);
#1491=EDGE_CURVE('',#1229,#1229,#1047,.T.);
#1492=EDGE_CURVE('',#1229,#1228,#782,.T.);
#1493=EDGE_CURVE('',#1230,#1231,#783,.T.);
#1494=EDGE_CURVE('',#1231,#1232,#784,.T.);
#1495=EDGE_CURVE('',#1232,#1233,#785,.T.);
#1496=EDGE_CURVE('',#1230,#1233,#786,.T.);
#1497=EDGE_CURVE('',#1231,#1234,#787,.T.);
#1498=EDGE_CURVE('',#1234,#1235,#788,.T.);
#1499=EDGE_CURVE('',#1235,#1232,#789,.T.);
#1500=EDGE_CURVE('',#1234,#1236,#790,.T.);
#1501=EDGE_CURVE('',#1236,#1237,#791,.T.);
#1502=EDGE_CURVE('',#1237,#1235,#792,.T.);
#1503=EDGE_CURVE('',#1236,#1238,#793,.T.);
#1504=EDGE_CURVE('',#1238,#1239,#794,.T.);
#1505=EDGE_CURVE('',#1239,#1237,#795,.T.);
#1506=EDGE_CURVE('',#1238,#1240,#796,.T.);
#1507=EDGE_CURVE('',#1240,#1241,#797,.T.);
#1508=EDGE_CURVE('',#1241,#1239,#798,.T.);
#1509=EDGE_CURVE('',#1240,#1230,#799,.T.);
#1510=EDGE_CURVE('',#1233,#1241,#800,.T.);
#1511=EDGE_CURVE('',#1242,#1242,#1048,.T.);
#1512=EDGE_CURVE('',#1242,#1243,#801,.T.);
#1513=EDGE_CURVE('',#1243,#1243,#1049,.T.);
#1514=EDGE_CURVE('',#1244,#1244,#1050,.T.);
#1515=EDGE_CURVE('',#1245,#1245,#1051,.T.);
#1516=EDGE_CURVE('',#1245,#1246,#802,.T.);
#1517=EDGE_CURVE('',#1246,#1246,#1052,.T.);
#1518=EDGE_CURVE('',#1247,#1247,#1053,.T.);
#1519=EDGE_CURVE('',#1248,#1248,#1054,.T.);
#1520=EDGE_CURVE('',#1249,#1249,#1055,.T.);
#1521=EDGE_CURVE('',#1247,#1248,#803,.T.);
#1522=EDGE_CURVE('',#1249,#1250,#804,.T.);
#1523=EDGE_CURVE('',#1250,#1250,#1056,.T.);
#1524=EDGE_CURVE('',#1251,#1251,#1057,.T.);
#1525=EDGE_CURVE('',#1251,#1244,#805,.T.);
#1526=EDGE_CURVE('',#1252,#1252,#1058,.T.);
#1527=EDGE_CURVE('',#1252,#1253,#806,.T.);
#1528=EDGE_CURVE('',#1253,#1253,#1059,.T.);
#1529=EDGE_CURVE('',#1254,#1254,#1060,.T.);
#1530=EDGE_CURVE('',#1254,#1255,#807,.T.);
#1531=EDGE_CURVE('',#1255,#1255,#1061,.T.);
#1532=EDGE_CURVE('',#1256,#1257,#808,.T.);
#1533=EDGE_CURVE('',#1258,#1256,#1062,.T.);
#1534=EDGE_CURVE('',#1259,#1258,#809,.T.);
#1535=EDGE_CURVE('',#1257,#1259,#1063,.T.);
#1536=EDGE_CURVE('',#1258,#1260,#1064,.T.);
#1537=EDGE_CURVE('',#1261,#1260,#134,.T.);
#1538=EDGE_CURVE('',#1259,#1261,#1065,.T.);
#1539=EDGE_CURVE('',#1262,#1256,#1066,.T.);
#1540=EDGE_CURVE('',#1260,#1262,#12,.T.);
#1541=EDGE_CURVE('',#1263,#1263,#1067,.T.);
#1542=EDGE_CURVE('',#1264,#1264,#1068,.T.);
#1543=EDGE_CURVE('',#1264,#1265,#810,.T.);
#1544=EDGE_CURVE('',#1265,#1265,#1069,.T.);
#1545=EDGE_CURVE('',#1263,#1266,#811,.T.);
#1546=EDGE_CURVE('',#1266,#1266,#1070,.T.);
#1547=EDGE_CURVE('',#1267,#1257,#1071,.T.);
#1548=EDGE_CURVE('',#1262,#1267,#135,.T.);
#1549=EDGE_CURVE('',#1261,#1267,#13,.T.);
#1550=ORIENTED_EDGE('',*,*,#1268,.F.);
#1551=ORIENTED_EDGE('',*,*,#1269,.T.);
#1552=ORIENTED_EDGE('',*,*,#1270,.F.);
#1553=ORIENTED_EDGE('',*,*,#1269,.F.);
#1554=ORIENTED_EDGE('',*,*,#1271,.F.);
#1555=ORIENTED_EDGE('',*,*,#1272,.T.);
#1556=ORIENTED_EDGE('',*,*,#1273,.F.);
#1557=ORIENTED_EDGE('',*,*,#1272,.F.);
#1558=ORIENTED_EDGE('',*,*,#1274,.F.);
#1559=ORIENTED_EDGE('',*,*,#1275,.T.);
#1560=ORIENTED_EDGE('',*,*,#1276,.F.);
#1561=ORIENTED_EDGE('',*,*,#1275,.F.);
#1562=ORIENTED_EDGE('',*,*,#1277,.F.);
#1563=ORIENTED_EDGE('',*,*,#1278,.T.);
#1564=ORIENTED_EDGE('',*,*,#1279,.F.);
#1565=ORIENTED_EDGE('',*,*,#1278,.F.);
#1566=ORIENTED_EDGE('',*,*,#1280,.F.);
#1567=ORIENTED_EDGE('',*,*,#1281,.T.);
#1568=ORIENTED_EDGE('',*,*,#1282,.F.);
#1569=ORIENTED_EDGE('',*,*,#1281,.F.);
#1570=ORIENTED_EDGE('',*,*,#1280,.T.);
#1571=ORIENTED_EDGE('',*,*,#1283,.F.);
#1572=ORIENTED_EDGE('',*,*,#1284,.T.);
#1573=ORIENTED_EDGE('',*,*,#1285,.F.);
#1574=ORIENTED_EDGE('',*,*,#1284,.F.);
#1575=ORIENTED_EDGE('',*,*,#1283,.T.);
#1576=ORIENTED_EDGE('',*,*,#1286,.F.);
#1577=ORIENTED_EDGE('',*,*,#1287,.T.);
#1578=ORIENTED_EDGE('',*,*,#1288,.F.);
#1579=ORIENTED_EDGE('',*,*,#1287,.F.);
#1580=ORIENTED_EDGE('',*,*,#1286,.T.);
#1581=ORIENTED_EDGE('',*,*,#1289,.F.);
#1582=ORIENTED_EDGE('',*,*,#1290,.T.);
#1583=ORIENTED_EDGE('',*,*,#1291,.F.);
#1584=ORIENTED_EDGE('',*,*,#1290,.F.);
#1585=ORIENTED_EDGE('',*,*,#1289,.T.);
#1586=ORIENTED_EDGE('',*,*,#1292,.F.);
#1587=ORIENTED_EDGE('',*,*,#1293,.T.);
#1588=ORIENTED_EDGE('',*,*,#1294,.T.);
#1589=ORIENTED_EDGE('',*,*,#1293,.F.);
#1590=ORIENTED_EDGE('',*,*,#1294,.F.);
#1591=ORIENTED_EDGE('',*,*,#1295,.F.);
#1592=ORIENTED_EDGE('',*,*,#1296,.T.);
#1593=ORIENTED_EDGE('',*,*,#1297,.T.);
#1594=ORIENTED_EDGE('',*,*,#1296,.F.);
#1595=ORIENTED_EDGE('',*,*,#1297,.F.);
#1596=ORIENTED_EDGE('',*,*,#1298,.F.);
#1597=ORIENTED_EDGE('',*,*,#1299,.T.);
#1598=ORIENTED_EDGE('',*,*,#1300,.T.);
#1599=ORIENTED_EDGE('',*,*,#1299,.F.);
#1600=ORIENTED_EDGE('',*,*,#1300,.F.);
#1601=ORIENTED_EDGE('',*,*,#1301,.F.);
#1602=ORIENTED_EDGE('',*,*,#1302,.T.);
#1603=ORIENTED_EDGE('',*,*,#1303,.T.);
#1604=ORIENTED_EDGE('',*,*,#1302,.F.);
#1605=ORIENTED_EDGE('',*,*,#1303,.F.);
#1606=ORIENTED_EDGE('',*,*,#1304,.T.);
#1607=ORIENTED_EDGE('',*,*,#1305,.F.);
#1608=ORIENTED_EDGE('',*,*,#1279,.T.);
#1609=ORIENTED_EDGE('',*,*,#1276,.T.);
#1610=ORIENTED_EDGE('',*,*,#1273,.T.);
#1611=ORIENTED_EDGE('',*,*,#1270,.T.);
#1612=ORIENTED_EDGE('',*,*,#1306,.F.);
#1613=ORIENTED_EDGE('',*,*,#1307,.F.);
#1614=ORIENTED_EDGE('',*,*,#1277,.T.);
#1615=ORIENTED_EDGE('',*,*,#1274,.T.);
#1616=ORIENTED_EDGE('',*,*,#1271,.T.);
#1617=ORIENTED_EDGE('',*,*,#1268,.T.);
#1618=ORIENTED_EDGE('',*,*,#1304,.F.);
#1619=ORIENTED_EDGE('',*,*,#1308,.T.);
#1620=ORIENTED_EDGE('',*,*,#1306,.T.);
#1621=ORIENTED_EDGE('',*,*,#1308,.F.);
#1622=ORIENTED_EDGE('',*,*,#1307,.T.);
#1623=ORIENTED_EDGE('',*,*,#1309,.T.);
#1624=ORIENTED_EDGE('',*,*,#1310,.T.);
#1625=ORIENTED_EDGE('',*,*,#1309,.F.);
#1626=ORIENTED_EDGE('',*,*,#1311,.F.);
#1627=ORIENTED_EDGE('',*,*,#1312,.T.);
#1628=ORIENTED_EDGE('',*,*,#1313,.T.);
#1629=ORIENTED_EDGE('',*,*,#1312,.F.);
#1630=ORIENTED_EDGE('',*,*,#1314,.F.);
#1631=ORIENTED_EDGE('',*,*,#1315,.T.);
#1632=ORIENTED_EDGE('',*,*,#1305,.T.);
#1633=ORIENTED_EDGE('',*,*,#1315,.F.);
#1634=ORIENTED_EDGE('',*,*,#1314,.T.);
#1635=ORIENTED_EDGE('',*,*,#1311,.T.);
#1636=ORIENTED_EDGE('',*,*,#1291,.T.);
#1637=ORIENTED_EDGE('',*,*,#1288,.T.);
#1638=ORIENTED_EDGE('',*,*,#1285,.T.);
#1639=ORIENTED_EDGE('',*,*,#1282,.T.);
#1640=ORIENTED_EDGE('',*,*,#1310,.F.);
#1641=ORIENTED_EDGE('',*,*,#1313,.F.);
#1642=ORIENTED_EDGE('',*,*,#1301,.T.);
#1643=ORIENTED_EDGE('',*,*,#1298,.T.);
#1644=ORIENTED_EDGE('',*,*,#1295,.T.);
#1645=ORIENTED_EDGE('',*,*,#1292,.T.);
#1646=ORIENTED_EDGE('',*,*,#1316,.F.);
#1647=ORIENTED_EDGE('',*,*,#1317,.F.);
#1648=ORIENTED_EDGE('',*,*,#1318,.T.);
#1649=ORIENTED_EDGE('',*,*,#1319,.F.);
#1650=ORIENTED_EDGE('',*,*,#1320,.F.);
#1651=ORIENTED_EDGE('',*,*,#1318,.F.);
#1652=ORIENTED_EDGE('',*,*,#1319,.T.);
#1653=ORIENTED_EDGE('',*,*,#1320,.T.);
#1654=ORIENTED_EDGE('',*,*,#1321,.T.);
#1655=ORIENTED_EDGE('',*,*,#1322,.T.);
#1656=ORIENTED_EDGE('',*,*,#1321,.F.);
#1657=ORIENTED_EDGE('',*,*,#1323,.T.);
#1658=ORIENTED_EDGE('',*,*,#1324,.T.);
#1659=ORIENTED_EDGE('',*,*,#1325,.F.);
#1660=ORIENTED_EDGE('',*,*,#1324,.F.);
#1661=ORIENTED_EDGE('',*,*,#1325,.T.);
#1662=ORIENTED_EDGE('',*,*,#1326,.T.);
#1663=ORIENTED_EDGE('',*,*,#1327,.F.);
#1664=ORIENTED_EDGE('',*,*,#1326,.F.);
#1665=ORIENTED_EDGE('',*,*,#1322,.F.);
#1666=ORIENTED_EDGE('',*,*,#1327,.T.);
#1667=ORIENTED_EDGE('',*,*,#1328,.F.);
#1668=ORIENTED_EDGE('',*,*,#1329,.T.);
#1669=ORIENTED_EDGE('',*,*,#1316,.T.);
#1670=ORIENTED_EDGE('',*,*,#1317,.T.);
#1671=ORIENTED_EDGE('',*,*,#1329,.F.);
#1672=ORIENTED_EDGE('',*,*,#1328,.T.);
#1673=ORIENTED_EDGE('',*,*,#1330,.F.);
#1674=ORIENTED_EDGE('',*,*,#1330,.T.);
#1675=ORIENTED_EDGE('',*,*,#1331,.T.);
#1676=ORIENTED_EDGE('',*,*,#1323,.F.);
#1677=ORIENTED_EDGE('',*,*,#1331,.F.);
#1678=ORIENTED_EDGE('',*,*,#1332,.F.);
#1679=ORIENTED_EDGE('',*,*,#1333,.F.);
#1680=ORIENTED_EDGE('',*,*,#1334,.T.);
#1681=ORIENTED_EDGE('',*,*,#1335,.F.);
#1682=ORIENTED_EDGE('',*,*,#1336,.F.);
#1683=ORIENTED_EDGE('',*,*,#1334,.F.);
#1684=ORIENTED_EDGE('',*,*,#1337,.T.);
#1685=ORIENTED_EDGE('',*,*,#1338,.T.);
#1686=ORIENTED_EDGE('',*,*,#1335,.T.);
#1687=ORIENTED_EDGE('',*,*,#1336,.T.);
#1688=ORIENTED_EDGE('',*,*,#1338,.F.);
#1689=ORIENTED_EDGE('',*,*,#1339,.F.);
#1690=ORIENTED_EDGE('',*,*,#1340,.T.);
#1691=ORIENTED_EDGE('',*,*,#1341,.F.);
#1692=ORIENTED_EDGE('',*,*,#1342,.T.);
#1693=ORIENTED_EDGE('',*,*,#1339,.T.);
#1694=ORIENTED_EDGE('',*,*,#1342,.F.);
#1695=ORIENTED_EDGE('',*,*,#1343,.F.);
#1696=ORIENTED_EDGE('',*,*,#1344,.T.);
#1697=ORIENTED_EDGE('',*,*,#1341,.T.);
#1698=ORIENTED_EDGE('',*,*,#1344,.F.);
#1699=ORIENTED_EDGE('',*,*,#1345,.F.);
#1700=ORIENTED_EDGE('',*,*,#1346,.T.);
#1701=ORIENTED_EDGE('',*,*,#1343,.T.);
#1702=ORIENTED_EDGE('',*,*,#1346,.F.);
#1703=ORIENTED_EDGE('',*,*,#1345,.T.);
#1704=ORIENTED_EDGE('',*,*,#1337,.F.);
#1705=ORIENTED_EDGE('',*,*,#1332,.T.);
#1706=ORIENTED_EDGE('',*,*,#1333,.T.);
#1707=ORIENTED_EDGE('',*,*,#1347,.T.);
#1708=ORIENTED_EDGE('',*,*,#1340,.F.);
#1709=ORIENTED_EDGE('',*,*,#1347,.F.);
#1710=ORIENTED_EDGE('',*,*,#1348,.T.);
#1711=ORIENTED_EDGE('',*,*,#1348,.F.);
#1712=ORIENTED_EDGE('',*,*,#1349,.T.);
#1713=ORIENTED_EDGE('',*,*,#1349,.F.);
#1714=ORIENTED_EDGE('',*,*,#1350,.T.);
#1715=ORIENTED_EDGE('',*,*,#1350,.F.);
#1716=ORIENTED_EDGE('',*,*,#1351,.T.);
#1717=ORIENTED_EDGE('',*,*,#1351,.F.);
#1718=ORIENTED_EDGE('',*,*,#1352,.T.);
#1719=ORIENTED_EDGE('',*,*,#1352,.F.);
#1720=ORIENTED_EDGE('',*,*,#1353,.T.);
#1721=ORIENTED_EDGE('',*,*,#1353,.F.);
#1722=ORIENTED_EDGE('',*,*,#1354,.T.);
#1723=ORIENTED_EDGE('',*,*,#1354,.F.);
#1724=ORIENTED_EDGE('',*,*,#1355,.T.);
#1725=ORIENTED_EDGE('',*,*,#1355,.F.);
#1726=ORIENTED_EDGE('',*,*,#1356,.F.);
#1727=ORIENTED_EDGE('',*,*,#1357,.F.);
#1728=ORIENTED_EDGE('',*,*,#1358,.F.);
#1729=ORIENTED_EDGE('',*,*,#1359,.F.);
#1730=ORIENTED_EDGE('',*,*,#1358,.T.);
#1731=ORIENTED_EDGE('',*,*,#1360,.F.);
#1732=ORIENTED_EDGE('',*,*,#1361,.T.);
#1733=ORIENTED_EDGE('',*,*,#1362,.F.);
#1734=ORIENTED_EDGE('',*,*,#1363,.T.);
#1735=ORIENTED_EDGE('',*,*,#1364,.F.);
#1736=ORIENTED_EDGE('',*,*,#1365,.T.);
#1737=ORIENTED_EDGE('',*,*,#1366,.T.);
#1738=ORIENTED_EDGE('',*,*,#1367,.F.);
#1739=ORIENTED_EDGE('',*,*,#1366,.F.);
#1740=ORIENTED_EDGE('',*,*,#1368,.T.);
#1741=ORIENTED_EDGE('',*,*,#1369,.F.);
#1742=ORIENTED_EDGE('',*,*,#1370,.T.);
#1743=ORIENTED_EDGE('',*,*,#1371,.F.);
#1744=ORIENTED_EDGE('',*,*,#1372,.T.);
#1745=ORIENTED_EDGE('',*,*,#1373,.F.);
#1746=ORIENTED_EDGE('',*,*,#1374,.T.);
#1747=ORIENTED_EDGE('',*,*,#1375,.F.);
#1748=ORIENTED_EDGE('',*,*,#1376,.T.);
#1749=ORIENTED_EDGE('',*,*,#1377,.F.);
#1750=ORIENTED_EDGE('',*,*,#1357,.T.);
#1751=ORIENTED_EDGE('',*,*,#1378,.T.);
#1752=ORIENTED_EDGE('',*,*,#1379,.T.);
#1753=ORIENTED_EDGE('',*,*,#1360,.T.);
#1754=ORIENTED_EDGE('',*,*,#1380,.F.);
#1755=ORIENTED_EDGE('',*,*,#1381,.F.);
#1756=ORIENTED_EDGE('',*,*,#1361,.F.);
#1757=ORIENTED_EDGE('',*,*,#1379,.F.);
#1758=ORIENTED_EDGE('',*,*,#1381,.T.);
#1759=ORIENTED_EDGE('',*,*,#1382,.T.);
#1760=ORIENTED_EDGE('',*,*,#1383,.T.);
#1761=ORIENTED_EDGE('',*,*,#1362,.T.);
#1762=ORIENTED_EDGE('',*,*,#1384,.F.);
#1763=ORIENTED_EDGE('',*,*,#1385,.F.);
#1764=ORIENTED_EDGE('',*,*,#1363,.F.);
#1765=ORIENTED_EDGE('',*,*,#1383,.F.);
#1766=ORIENTED_EDGE('',*,*,#1385,.T.);
#1767=ORIENTED_EDGE('',*,*,#1386,.T.);
#1768=ORIENTED_EDGE('',*,*,#1387,.T.);
#1769=ORIENTED_EDGE('',*,*,#1364,.T.);
#1770=ORIENTED_EDGE('',*,*,#1388,.F.);
#1771=ORIENTED_EDGE('',*,*,#1389,.F.);
#1772=ORIENTED_EDGE('',*,*,#1368,.F.);
#1773=ORIENTED_EDGE('',*,*,#1365,.F.);
#1774=ORIENTED_EDGE('',*,*,#1387,.F.);
#1775=ORIENTED_EDGE('',*,*,#1390,.F.);
#1776=ORIENTED_EDGE('',*,*,#1389,.T.);
#1777=ORIENTED_EDGE('',*,*,#1391,.T.);
#1778=ORIENTED_EDGE('',*,*,#1392,.T.);
#1779=ORIENTED_EDGE('',*,*,#1369,.T.);
#1780=ORIENTED_EDGE('',*,*,#1393,.F.);
#1781=ORIENTED_EDGE('',*,*,#1394,.F.);
#1782=ORIENTED_EDGE('',*,*,#1370,.F.);
#1783=ORIENTED_EDGE('',*,*,#1392,.F.);
#1784=ORIENTED_EDGE('',*,*,#1394,.T.);
#1785=ORIENTED_EDGE('',*,*,#1395,.T.);
#1786=ORIENTED_EDGE('',*,*,#1396,.T.);
#1787=ORIENTED_EDGE('',*,*,#1371,.T.);
#1788=ORIENTED_EDGE('',*,*,#1397,.F.);
#1789=ORIENTED_EDGE('',*,*,#1398,.F.);
#1790=ORIENTED_EDGE('',*,*,#1372,.F.);
#1791=ORIENTED_EDGE('',*,*,#1396,.F.);
#1792=ORIENTED_EDGE('',*,*,#1398,.T.);
#1793=ORIENTED_EDGE('',*,*,#1399,.T.);
#1794=ORIENTED_EDGE('',*,*,#1400,.T.);
#1795=ORIENTED_EDGE('',*,*,#1373,.T.);
#1796=ORIENTED_EDGE('',*,*,#1374,.F.);
#1797=ORIENTED_EDGE('',*,*,#1400,.F.);
#1798=ORIENTED_EDGE('',*,*,#1401,.F.);
#1799=ORIENTED_EDGE('',*,*,#1402,.F.);
#1800=ORIENTED_EDGE('',*,*,#1403,.F.);
#1801=ORIENTED_EDGE('',*,*,#1404,.T.);
#1802=ORIENTED_EDGE('',*,*,#1390,.T.);
#1803=ORIENTED_EDGE('',*,*,#1386,.F.);
#1804=ORIENTED_EDGE('',*,*,#1384,.T.);
#1805=ORIENTED_EDGE('',*,*,#1382,.F.);
#1806=ORIENTED_EDGE('',*,*,#1380,.T.);
#1807=ORIENTED_EDGE('',*,*,#1378,.F.);
#1808=ORIENTED_EDGE('',*,*,#1356,.T.);
#1809=ORIENTED_EDGE('',*,*,#1405,.F.);
#1810=ORIENTED_EDGE('',*,*,#1406,.T.);
#1811=ORIENTED_EDGE('',*,*,#1407,.F.);
#1812=ORIENTED_EDGE('',*,*,#1401,.T.);
#1813=ORIENTED_EDGE('',*,*,#1399,.F.);
#1814=ORIENTED_EDGE('',*,*,#1397,.T.);
#1815=ORIENTED_EDGE('',*,*,#1395,.F.);
#1816=ORIENTED_EDGE('',*,*,#1393,.T.);
#1817=ORIENTED_EDGE('',*,*,#1391,.F.);
#1818=ORIENTED_EDGE('',*,*,#1388,.T.);
#1819=ORIENTED_EDGE('',*,*,#1404,.F.);
#1820=ORIENTED_EDGE('',*,*,#1359,.T.);
#1821=ORIENTED_EDGE('',*,*,#1377,.T.);
#1822=ORIENTED_EDGE('',*,*,#1408,.T.);
#1823=ORIENTED_EDGE('',*,*,#1405,.T.);
#1824=ORIENTED_EDGE('',*,*,#1376,.F.);
#1825=ORIENTED_EDGE('',*,*,#1409,.F.);
#1826=ORIENTED_EDGE('',*,*,#1406,.F.);
#1827=ORIENTED_EDGE('',*,*,#1408,.F.);
#1828=ORIENTED_EDGE('',*,*,#1367,.T.);
#1829=ORIENTED_EDGE('',*,*,#1403,.T.);
#1830=ORIENTED_EDGE('',*,*,#1402,.T.);
#1831=ORIENTED_EDGE('',*,*,#1407,.T.);
#1832=ORIENTED_EDGE('',*,*,#1409,.T.);
#1833=ORIENTED_EDGE('',*,*,#1375,.T.);
#1834=ORIENTED_EDGE('',*,*,#1410,.F.);
#1835=ORIENTED_EDGE('',*,*,#1411,.T.);
#1836=ORIENTED_EDGE('',*,*,#1412,.F.);
#1837=ORIENTED_EDGE('',*,*,#1413,.T.);
#1838=ORIENTED_EDGE('',*,*,#1410,.T.);
#1839=ORIENTED_EDGE('',*,*,#1413,.F.);
#1840=ORIENTED_EDGE('',*,*,#1412,.T.);
#1841=ORIENTED_EDGE('',*,*,#1414,.F.);
#1842=ORIENTED_EDGE('',*,*,#1414,.T.);
#1843=ORIENTED_EDGE('',*,*,#1415,.T.);
#1844=ORIENTED_EDGE('',*,*,#1411,.F.);
#1845=ORIENTED_EDGE('',*,*,#1415,.F.);
#1846=ORIENTED_EDGE('',*,*,#1416,.F.);
#1847=ORIENTED_EDGE('',*,*,#1417,.T.);
#1848=ORIENTED_EDGE('',*,*,#1418,.F.);
#1849=ORIENTED_EDGE('',*,*,#1419,.T.);
#1850=ORIENTED_EDGE('',*,*,#1416,.T.);
#1851=ORIENTED_EDGE('',*,*,#1419,.F.);
#1852=ORIENTED_EDGE('',*,*,#1418,.T.);
#1853=ORIENTED_EDGE('',*,*,#1420,.F.);
#1854=ORIENTED_EDGE('',*,*,#1420,.T.);
#1855=ORIENTED_EDGE('',*,*,#1421,.T.);
#1856=ORIENTED_EDGE('',*,*,#1417,.F.);
#1857=ORIENTED_EDGE('',*,*,#1421,.F.);
#1858=ORIENTED_EDGE('',*,*,#1422,.F.);
#1859=ORIENTED_EDGE('',*,*,#1423,.T.);
#1860=ORIENTED_EDGE('',*,*,#1424,.T.);
#1861=ORIENTED_EDGE('',*,*,#1423,.F.);
#1862=ORIENTED_EDGE('',*,*,#1425,.F.);
#1863=ORIENTED_EDGE('',*,*,#1426,.T.);
#1864=ORIENTED_EDGE('',*,*,#1427,.T.);
#1865=ORIENTED_EDGE('',*,*,#1426,.F.);
#1866=ORIENTED_EDGE('',*,*,#1425,.T.);
#1867=ORIENTED_EDGE('',*,*,#1422,.T.);
#1868=ORIENTED_EDGE('',*,*,#1427,.F.);
#1869=ORIENTED_EDGE('',*,*,#1424,.F.);
#1870=ORIENTED_EDGE('',*,*,#1428,.F.);
#1871=ORIENTED_EDGE('',*,*,#1429,.T.);
#1872=ORIENTED_EDGE('',*,*,#1430,.F.);
#1873=ORIENTED_EDGE('',*,*,#1429,.F.);
#1874=ORIENTED_EDGE('',*,*,#1431,.F.);
#1875=ORIENTED_EDGE('',*,*,#1432,.T.);
#1876=ORIENTED_EDGE('',*,*,#1433,.F.);
#1877=ORIENTED_EDGE('',*,*,#1432,.F.);
#1878=ORIENTED_EDGE('',*,*,#1434,.F.);
#1879=ORIENTED_EDGE('',*,*,#1435,.T.);
#1880=ORIENTED_EDGE('',*,*,#1436,.F.);
#1881=ORIENTED_EDGE('',*,*,#1435,.F.);
#1882=ORIENTED_EDGE('',*,*,#1437,.F.);
#1883=ORIENTED_EDGE('',*,*,#1438,.T.);
#1884=ORIENTED_EDGE('',*,*,#1439,.F.);
#1885=ORIENTED_EDGE('',*,*,#1438,.F.);
#1886=ORIENTED_EDGE('',*,*,#1440,.F.);
#1887=ORIENTED_EDGE('',*,*,#1441,.T.);
#1888=ORIENTED_EDGE('',*,*,#1442,.F.);
#1889=ORIENTED_EDGE('',*,*,#1441,.F.);
#1890=ORIENTED_EDGE('',*,*,#1440,.T.);
#1891=ORIENTED_EDGE('',*,*,#1443,.T.);
#1892=ORIENTED_EDGE('',*,*,#1444,.F.);
#1893=ORIENTED_EDGE('',*,*,#1445,.T.);
#1894=ORIENTED_EDGE('',*,*,#1446,.T.);
#1895=ORIENTED_EDGE('',*,*,#1445,.F.);
#1896=ORIENTED_EDGE('',*,*,#1446,.F.);
#1897=ORIENTED_EDGE('',*,*,#1447,.F.);
#1898=ORIENTED_EDGE('',*,*,#1443,.F.);
#1899=ORIENTED_EDGE('',*,*,#1448,.T.);
#1900=ORIENTED_EDGE('',*,*,#1447,.T.);
#1901=ORIENTED_EDGE('',*,*,#1448,.F.);
#1902=ORIENTED_EDGE('',*,*,#1449,.F.);
#1903=ORIENTED_EDGE('',*,*,#1450,.T.);
#1904=ORIENTED_EDGE('',*,*,#1451,.T.);
#1905=ORIENTED_EDGE('',*,*,#1450,.F.);
#1906=ORIENTED_EDGE('',*,*,#1449,.T.);
#1907=ORIENTED_EDGE('',*,*,#1442,.T.);
#1908=ORIENTED_EDGE('',*,*,#1439,.T.);
#1909=ORIENTED_EDGE('',*,*,#1436,.T.);
#1910=ORIENTED_EDGE('',*,*,#1433,.T.);
#1911=ORIENTED_EDGE('',*,*,#1430,.T.);
#1912=ORIENTED_EDGE('',*,*,#1451,.F.);
#1913=ORIENTED_EDGE('',*,*,#1444,.T.);
#1914=ORIENTED_EDGE('',*,*,#1437,.T.);
#1915=ORIENTED_EDGE('',*,*,#1434,.T.);
#1916=ORIENTED_EDGE('',*,*,#1431,.T.);
#1917=ORIENTED_EDGE('',*,*,#1428,.T.);
#1918=ORIENTED_EDGE('',*,*,#1452,.F.);
#1919=ORIENTED_EDGE('',*,*,#1453,.T.);
#1920=ORIENTED_EDGE('',*,*,#1454,.T.);
#1921=ORIENTED_EDGE('',*,*,#1453,.F.);
#1922=ORIENTED_EDGE('',*,*,#1455,.F.);
#1923=ORIENTED_EDGE('',*,*,#1456,.T.);
#1924=ORIENTED_EDGE('',*,*,#1457,.T.);
#1925=ORIENTED_EDGE('',*,*,#1456,.F.);
#1926=ORIENTED_EDGE('',*,*,#1455,.T.);
#1927=ORIENTED_EDGE('',*,*,#1452,.T.);
#1928=ORIENTED_EDGE('',*,*,#1457,.F.);
#1929=ORIENTED_EDGE('',*,*,#1454,.F.);
#1930=ORIENTED_EDGE('',*,*,#1458,.F.);
#1931=ORIENTED_EDGE('',*,*,#1459,.T.);
#1932=ORIENTED_EDGE('',*,*,#1460,.F.);
#1933=ORIENTED_EDGE('',*,*,#1459,.F.);
#1934=ORIENTED_EDGE('',*,*,#1461,.F.);
#1935=ORIENTED_EDGE('',*,*,#1462,.T.);
#1936=ORIENTED_EDGE('',*,*,#1463,.F.);
#1937=ORIENTED_EDGE('',*,*,#1462,.F.);
#1938=ORIENTED_EDGE('',*,*,#1464,.F.);
#1939=ORIENTED_EDGE('',*,*,#1465,.T.);
#1940=ORIENTED_EDGE('',*,*,#1466,.F.);
#1941=ORIENTED_EDGE('',*,*,#1465,.F.);
#1942=ORIENTED_EDGE('',*,*,#1467,.F.);
#1943=ORIENTED_EDGE('',*,*,#1468,.T.);
#1944=ORIENTED_EDGE('',*,*,#1469,.F.);
#1945=ORIENTED_EDGE('',*,*,#1468,.F.);
#1946=ORIENTED_EDGE('',*,*,#1470,.F.);
#1947=ORIENTED_EDGE('',*,*,#1471,.T.);
#1948=ORIENTED_EDGE('',*,*,#1472,.T.);
#1949=ORIENTED_EDGE('',*,*,#1471,.F.);
#1950=ORIENTED_EDGE('',*,*,#1472,.F.);
#1951=ORIENTED_EDGE('',*,*,#1473,.F.);
#1952=ORIENTED_EDGE('',*,*,#1474,.F.);
#1953=ORIENTED_EDGE('',*,*,#1475,.T.);
#1954=ORIENTED_EDGE('',*,*,#1473,.T.);
#1955=ORIENTED_EDGE('',*,*,#1475,.F.);
#1956=ORIENTED_EDGE('',*,*,#1476,.F.);
#1957=ORIENTED_EDGE('',*,*,#1477,.T.);
#1958=ORIENTED_EDGE('',*,*,#1478,.T.);
#1959=ORIENTED_EDGE('',*,*,#1477,.F.);
#1960=ORIENTED_EDGE('',*,*,#1476,.T.);
#1961=ORIENTED_EDGE('',*,*,#1474,.T.);
#1962=ORIENTED_EDGE('',*,*,#1469,.T.);
#1963=ORIENTED_EDGE('',*,*,#1466,.T.);
#1964=ORIENTED_EDGE('',*,*,#1463,.T.);
#1965=ORIENTED_EDGE('',*,*,#1460,.T.);
#1966=ORIENTED_EDGE('',*,*,#1478,.F.);
#1967=ORIENTED_EDGE('',*,*,#1470,.T.);
#1968=ORIENTED_EDGE('',*,*,#1467,.T.);
#1969=ORIENTED_EDGE('',*,*,#1464,.T.);
#1970=ORIENTED_EDGE('',*,*,#1461,.T.);
#1971=ORIENTED_EDGE('',*,*,#1458,.T.);
#1972=ORIENTED_EDGE('',*,*,#1479,.F.);
#1973=ORIENTED_EDGE('',*,*,#1480,.F.);
#1974=ORIENTED_EDGE('',*,*,#1481,.T.);
#1975=ORIENTED_EDGE('',*,*,#1479,.T.);
#1976=ORIENTED_EDGE('',*,*,#1481,.F.);
#1977=ORIENTED_EDGE('',*,*,#1482,.F.);
#1978=ORIENTED_EDGE('',*,*,#1483,.T.);
#1979=ORIENTED_EDGE('',*,*,#1480,.T.);
#1980=ORIENTED_EDGE('',*,*,#1483,.F.);
#1981=ORIENTED_EDGE('',*,*,#1484,.F.);
#1982=ORIENTED_EDGE('',*,*,#1485,.T.);
#1983=ORIENTED_EDGE('',*,*,#1482,.T.);
#1984=ORIENTED_EDGE('',*,*,#1485,.F.);
#1985=ORIENTED_EDGE('',*,*,#1484,.T.);
#1986=ORIENTED_EDGE('',*,*,#1486,.F.);
#1987=ORIENTED_EDGE('',*,*,#1487,.F.);
#1988=ORIENTED_EDGE('',*,*,#1488,.T.);
#1989=ORIENTED_EDGE('',*,*,#1486,.T.);
#1990=ORIENTED_EDGE('',*,*,#1488,.F.);
#1991=ORIENTED_EDGE('',*,*,#1489,.F.);
#1992=ORIENTED_EDGE('',*,*,#1490,.T.);
#1993=ORIENTED_EDGE('',*,*,#1487,.T.);
#1994=ORIENTED_EDGE('',*,*,#1490,.F.);
#1995=ORIENTED_EDGE('',*,*,#1491,.F.);
#1996=ORIENTED_EDGE('',*,*,#1492,.T.);
#1997=ORIENTED_EDGE('',*,*,#1489,.T.);
#1998=ORIENTED_EDGE('',*,*,#1492,.F.);
#1999=ORIENTED_EDGE('',*,*,#1491,.T.);
#2000=ORIENTED_EDGE('',*,*,#1493,.T.);
#2001=ORIENTED_EDGE('',*,*,#1494,.T.);
#2002=ORIENTED_EDGE('',*,*,#1495,.T.);
#2003=ORIENTED_EDGE('',*,*,#1496,.F.);
#2004=ORIENTED_EDGE('',*,*,#1497,.T.);
#2005=ORIENTED_EDGE('',*,*,#1498,.T.);
#2006=ORIENTED_EDGE('',*,*,#1499,.T.);
#2007=ORIENTED_EDGE('',*,*,#1494,.F.);
#2008=ORIENTED_EDGE('',*,*,#1500,.T.);
#2009=ORIENTED_EDGE('',*,*,#1501,.T.);
#2010=ORIENTED_EDGE('',*,*,#1502,.T.);
#2011=ORIENTED_EDGE('',*,*,#1498,.F.);
#2012=ORIENTED_EDGE('',*,*,#1503,.T.);
#2013=ORIENTED_EDGE('',*,*,#1504,.T.);
#2014=ORIENTED_EDGE('',*,*,#1505,.T.);
#2015=ORIENTED_EDGE('',*,*,#1501,.F.);
#2016=ORIENTED_EDGE('',*,*,#1506,.T.);
#2017=ORIENTED_EDGE('',*,*,#1507,.T.);
#2018=ORIENTED_EDGE('',*,*,#1508,.T.);
#2019=ORIENTED_EDGE('',*,*,#1504,.F.);
#2020=ORIENTED_EDGE('',*,*,#1509,.T.);
#2021=ORIENTED_EDGE('',*,*,#1496,.T.);
#2022=ORIENTED_EDGE('',*,*,#1510,.T.);
#2023=ORIENTED_EDGE('',*,*,#1507,.F.);
#2024=ORIENTED_EDGE('',*,*,#1509,.F.);
#2025=ORIENTED_EDGE('',*,*,#1506,.F.);
#2026=ORIENTED_EDGE('',*,*,#1503,.F.);
#2027=ORIENTED_EDGE('',*,*,#1500,.F.);
#2028=ORIENTED_EDGE('',*,*,#1497,.F.);
#2029=ORIENTED_EDGE('',*,*,#1493,.F.);
#2030=ORIENTED_EDGE('',*,*,#1510,.F.);
#2031=ORIENTED_EDGE('',*,*,#1495,.F.);
#2032=ORIENTED_EDGE('',*,*,#1499,.F.);
#2033=ORIENTED_EDGE('',*,*,#1502,.F.);
#2034=ORIENTED_EDGE('',*,*,#1505,.F.);
#2035=ORIENTED_EDGE('',*,*,#1508,.F.);
#2036=ORIENTED_EDGE('',*,*,#1511,.F.);
#2037=ORIENTED_EDGE('',*,*,#1512,.T.);
#2038=ORIENTED_EDGE('',*,*,#1513,.T.);
#2039=ORIENTED_EDGE('',*,*,#1512,.F.);
#2040=ORIENTED_EDGE('',*,*,#1514,.F.);
#2041=ORIENTED_EDGE('',*,*,#1513,.F.);
#2042=ORIENTED_EDGE('',*,*,#1515,.F.);
#2043=ORIENTED_EDGE('',*,*,#1511,.T.);
#2044=ORIENTED_EDGE('',*,*,#1515,.T.);
#2045=ORIENTED_EDGE('',*,*,#1516,.T.);
#2046=ORIENTED_EDGE('',*,*,#1517,.T.);
#2047=ORIENTED_EDGE('',*,*,#1516,.F.);
#2048=ORIENTED_EDGE('',*,*,#1518,.T.);
#2049=ORIENTED_EDGE('',*,*,#1517,.F.);
#2050=ORIENTED_EDGE('',*,*,#1519,.F.);
#2051=ORIENTED_EDGE('',*,*,#1520,.F.);
#2052=ORIENTED_EDGE('',*,*,#1518,.F.);
#2053=ORIENTED_EDGE('',*,*,#1521,.T.);
#2054=ORIENTED_EDGE('',*,*,#1519,.T.);
#2055=ORIENTED_EDGE('',*,*,#1521,.F.);
#2056=ORIENTED_EDGE('',*,*,#1520,.T.);
#2057=ORIENTED_EDGE('',*,*,#1522,.T.);
#2058=ORIENTED_EDGE('',*,*,#1523,.T.);
#2059=ORIENTED_EDGE('',*,*,#1522,.F.);
#2060=ORIENTED_EDGE('',*,*,#1524,.F.);
#2061=ORIENTED_EDGE('',*,*,#1525,.T.);
#2062=ORIENTED_EDGE('',*,*,#1514,.T.);
#2063=ORIENTED_EDGE('',*,*,#1525,.F.);
#2064=ORIENTED_EDGE('',*,*,#1524,.T.);
#2065=ORIENTED_EDGE('',*,*,#1523,.F.);
#2066=ORIENTED_EDGE('',*,*,#1526,.F.);
#2067=ORIENTED_EDGE('',*,*,#1527,.T.);
#2068=ORIENTED_EDGE('',*,*,#1528,.T.);
#2069=ORIENTED_EDGE('',*,*,#1527,.F.);
#2070=ORIENTED_EDGE('',*,*,#1529,.F.);
#2071=ORIENTED_EDGE('',*,*,#1530,.T.);
#2072=ORIENTED_EDGE('',*,*,#1531,.T.);
#2073=ORIENTED_EDGE('',*,*,#1530,.F.);
#2074=ORIENTED_EDGE('',*,*,#1529,.T.);
#2075=ORIENTED_EDGE('',*,*,#1526,.T.);
#2076=ORIENTED_EDGE('',*,*,#1531,.F.);
#2077=ORIENTED_EDGE('',*,*,#1528,.F.);
#2078=ORIENTED_EDGE('',*,*,#1532,.F.);
#2079=ORIENTED_EDGE('',*,*,#1533,.F.);
#2080=ORIENTED_EDGE('',*,*,#1534,.F.);
#2081=ORIENTED_EDGE('',*,*,#1535,.F.);
#2082=ORIENTED_EDGE('',*,*,#1534,.T.);
#2083=ORIENTED_EDGE('',*,*,#1536,.T.);
#2084=ORIENTED_EDGE('',*,*,#1537,.F.);
#2085=ORIENTED_EDGE('',*,*,#1538,.F.);
#2086=ORIENTED_EDGE('',*,*,#1533,.T.);
#2087=ORIENTED_EDGE('',*,*,#1539,.F.);
#2088=ORIENTED_EDGE('',*,*,#1540,.F.);
#2089=ORIENTED_EDGE('',*,*,#1536,.F.);
#2090=ORIENTED_EDGE('',*,*,#1541,.T.);
#2091=ORIENTED_EDGE('',*,*,#1542,.T.);
#2092=ORIENTED_EDGE('',*,*,#1542,.F.);
#2093=ORIENTED_EDGE('',*,*,#1543,.T.);
#2094=ORIENTED_EDGE('',*,*,#1544,.F.);
#2095=ORIENTED_EDGE('',*,*,#1543,.F.);
#2096=ORIENTED_EDGE('',*,*,#1541,.F.);
#2097=ORIENTED_EDGE('',*,*,#1545,.T.);
#2098=ORIENTED_EDGE('',*,*,#1546,.F.);
#2099=ORIENTED_EDGE('',*,*,#1545,.F.);
#2100=ORIENTED_EDGE('',*,*,#1532,.T.);
#2101=ORIENTED_EDGE('',*,*,#1547,.F.);
#2102=ORIENTED_EDGE('',*,*,#1548,.F.);
#2103=ORIENTED_EDGE('',*,*,#1539,.T.);
#2104=ORIENTED_EDGE('',*,*,#1548,.T.);
#2105=ORIENTED_EDGE('',*,*,#1549,.F.);
#2106=ORIENTED_EDGE('',*,*,#1537,.T.);
#2107=ORIENTED_EDGE('',*,*,#1540,.T.);
#2108=ORIENTED_EDGE('',*,*,#1535,.T.);
#2109=ORIENTED_EDGE('',*,*,#1538,.T.);
#2110=ORIENTED_EDGE('',*,*,#1549,.T.);
#2111=ORIENTED_EDGE('',*,*,#1547,.T.);
#2112=ORIENTED_EDGE('',*,*,#1544,.T.);
#2113=ORIENTED_EDGE('',*,*,#1546,.T.);
#2114=CYLINDRICAL_SURFACE('',#2505,0.44);
#2115=CYLINDRICAL_SURFACE('',#2508,0.44);
#2116=CYLINDRICAL_SURFACE('',#2511,0.44);
#2117=CYLINDRICAL_SURFACE('',#2514,0.44);
#2118=CYLINDRICAL_SURFACE('',#2517,0.165);
#2119=CYLINDRICAL_SURFACE('',#2521,0.165);
#2120=CYLINDRICAL_SURFACE('',#2525,0.165);
#2121=CYLINDRICAL_SURFACE('',#2529,0.165);
#2122=CYLINDRICAL_SURFACE('',#2533,0.165);
#2123=CYLINDRICAL_SURFACE('',#2537,0.165);
#2124=CYLINDRICAL_SURFACE('',#2541,0.165);
#2125=CYLINDRICAL_SURFACE('',#2545,0.165);
#2126=CYLINDRICAL_SURFACE('',#2555,5.);
#2127=CYLINDRICAL_SURFACE('',#2556,3.5);
#2128=CYLINDRICAL_SURFACE('',#2558,2.35);
#2129=CYLINDRICAL_SURFACE('',#2561,3.5);
#2130=CYLINDRICAL_SURFACE('',#2573,1.63531);
#2131=CYLINDRICAL_SURFACE('',#2575,1.);
#2132=CYLINDRICAL_SURFACE('',#2581,1.63531);
#2133=CYLINDRICAL_SURFACE('',#2593,1.71469);
#2134=CYLINDRICAL_SURFACE('',#2600,2.35);
#2135=CYLINDRICAL_SURFACE('',#2605,1.71469);
#2136=CYLINDRICAL_SURFACE('',#2627,1.706752);
#2137=CYLINDRICAL_SURFACE('',#2667,1.643248);
#2138=CYLINDRICAL_SURFACE('',#2681,1.70469);
#2139=CYLINDRICAL_SURFACE('',#2685,1.65031);
#2140=CYLINDRICAL_SURFACE('',#2689,1.70469);
#2141=CYLINDRICAL_SURFACE('',#2693,1.65031);
#2142=CYLINDRICAL_SURFACE('',#2700,1.75);
#2143=CYLINDRICAL_SURFACE('',#2703,2.34);
#2144=CYLINDRICAL_SURFACE('',#2709,0.225);
#2145=CYLINDRICAL_SURFACE('',#2712,0.225);
#2146=CYLINDRICAL_SURFACE('',#2715,0.225);
#2147=CYLINDRICAL_SURFACE('',#2718,0.225);
#2148=CYLINDRICAL_SURFACE('',#2721,2.34);
#2149=CYLINDRICAL_SURFACE('',#2726,1.8);
#2150=CYLINDRICAL_SURFACE('',#2731,1.6);
#2151=CYLINDRICAL_SURFACE('',#2732,3.5);
#2152=CYLINDRICAL_SURFACE('',#2738,1.);
#2153=CYLINDRICAL_SURFACE('',#2741,1.8);
#2154=CYLINDRICAL_SURFACE('',#2747,0.225);
#2155=CYLINDRICAL_SURFACE('',#2750,0.225);
#2156=CYLINDRICAL_SURFACE('',#2753,0.225);
#2157=CYLINDRICAL_SURFACE('',#2756,0.225);
#2158=CYLINDRICAL_SURFACE('',#2759,2.34);
#2159=CYLINDRICAL_SURFACE('',#2764,1.8);
#2160=CYLINDRICAL_SURFACE('',#2766,3.5);
#2161=CYLINDRICAL_SURFACE('',#2776,0.35);
#2162=CYLINDRICAL_SURFACE('',#2784,0.1954);
#2163=CYLINDRICAL_SURFACE('',#2814,0.95);
#2164=CYLINDRICAL_SURFACE('',#2821,1.);
#2165=CYLINDRICAL_SURFACE('',#2828,1.2);
#2166=CYLINDRICAL_SURFACE('',#2829,1.);
#2167=CYLINDRICAL_SURFACE('',#2831,1.);
#2168=CYLINDRICAL_SURFACE('',#2836,1.01);
#2169=CYLINDRICAL_SURFACE('',#2839,1.35);
#2170=CYLINDRICAL_SURFACE('',#2845,0.95);
#2171=CYLINDRICAL_SURFACE('',#2848,0.1612);
#2172=CYLINDRICAL_SURFACE('',#2855,0.1);
#2173=CYLINDRICAL_SURFACE('',#2857,0.1);
#2174=CYLINDRICAL_SURFACE('',#2859,0.1612);
#2175=ADVANCED_FACE('',(#361),#2114,.F.);
#2176=ADVANCED_FACE('',(#362),#2115,.F.);
#2177=ADVANCED_FACE('',(#363),#2116,.F.);
#2178=ADVANCED_FACE('',(#364),#2117,.F.);
#2179=ADVANCED_FACE('',(#365),#2118,.F.);
#2180=ADVANCED_FACE('',(#366),#300,.T.);
#2181=ADVANCED_FACE('',(#367),#2119,.F.);
#2182=ADVANCED_FACE('',(#368),#301,.T.);
#2183=ADVANCED_FACE('',(#369),#2120,.F.);
#2184=ADVANCED_FACE('',(#370),#302,.T.);
#2185=ADVANCED_FACE('',(#371),#2121,.F.);
#2186=ADVANCED_FACE('',(#372),#303,.T.);
#2187=ADVANCED_FACE('',(#373),#2122,.F.);
#2188=ADVANCED_FACE('',(#374),#304,.F.);
#2189=ADVANCED_FACE('',(#375),#2123,.F.);
#2190=ADVANCED_FACE('',(#376),#305,.F.);
#2191=ADVANCED_FACE('',(#377),#2124,.F.);
#2192=ADVANCED_FACE('',(#378),#306,.F.);
#2193=ADVANCED_FACE('',(#379),#2125,.F.);
#2194=ADVANCED_FACE('',(#380),#307,.F.);
#2195=ADVANCED_FACE('',(#381,#233,#234,#235,#236,#237),#308,.T.);
#2196=ADVANCED_FACE('',(#382,#238,#239,#240,#241,#242),#309,.F.);
#2197=ADVANCED_FACE('',(#383),#2126,.T.);
#2198=ADVANCED_FACE('',(#384),#2127,.T.);
#2199=ADVANCED_FACE('',(#385),#2128,.F.);
#2200=ADVANCED_FACE('',(#386),#2129,.T.);
#2201=ADVANCED_FACE('',(#387,#243,#244,#245,#246,#247),#310,.T.);
#2202=ADVANCED_FACE('',(#388,#248,#249,#250,#251,#252),#311,.F.);
#2203=ADVANCED_FACE('',(#389),#160,.F.);
#2204=ADVANCED_FACE('',(#390),#2130,.T.);
#2205=ADVANCED_FACE('',(#391),#2131,.F.);
#2206=ADVANCED_FACE('',(#392),#152,.F.);
#2207=ADVANCED_FACE('',(#393,#253),#312,.T.);
#2208=ADVANCED_FACE('',(#394),#2132,.T.);
#2209=ADVANCED_FACE('',(#395,#254),#313,.T.);
#2210=ADVANCED_FACE('',(#396),#153,.F.);
#2211=ADVANCED_FACE('',(#397),#161,.F.);
#2212=ADVANCED_FACE('',(#398),#2133,.F.);
#2213=ADVANCED_FACE('',(#399,#255),#314,.T.);
#2214=ADVANCED_FACE('',(#400),#154,.T.);
#2215=ADVANCED_FACE('',(#401),#2134,.T.);
#2216=ADVANCED_FACE('',(#402),#155,.T.);
#2217=ADVANCED_FACE('',(#403,#256),#315,.T.);
#2218=ADVANCED_FACE('',(#404),#2135,.F.);
#2219=ADVANCED_FACE('',(#405),#136,.T.);
#2220=ADVANCED_FACE('',(#406),#137,.T.);
#2221=ADVANCED_FACE('',(#407),#138,.T.);
#2222=ADVANCED_FACE('',(#408),#139,.T.);
#2223=ADVANCED_FACE('',(#409),#140,.T.);
#2224=ADVANCED_FACE('',(#410),#141,.T.);
#2225=ADVANCED_FACE('',(#411),#142,.T.);
#2226=ADVANCED_FACE('',(#412),#143,.T.);
#2227=ADVANCED_FACE('',(#413),#144,.F.);
#2228=ADVANCED_FACE('',(#414),#2136,.T.);
#2229=ADVANCED_FACE('',(#415),#316,.T.);
#2230=ADVANCED_FACE('',(#416),#145,.F.);
#2231=ADVANCED_FACE('',(#417),#317,.T.);
#2232=ADVANCED_FACE('',(#418),#146,.F.);
#2233=ADVANCED_FACE('',(#419),#318,.T.);
#2234=ADVANCED_FACE('',(#420),#147,.F.);
#2235=ADVANCED_FACE('',(#421),#319,.T.);
#2236=ADVANCED_FACE('',(#422),#148,.F.);
#2237=ADVANCED_FACE('',(#423),#320,.T.);
#2238=ADVANCED_FACE('',(#424),#149,.F.);
#2239=ADVANCED_FACE('',(#425),#321,.T.);
#2240=ADVANCED_FACE('',(#426),#150,.F.);
#2241=ADVANCED_FACE('',(#427),#2137,.F.);
#2242=ADVANCED_FACE('',(#428),#322,.T.);
#2243=ADVANCED_FACE('',(#429),#151,.F.);
#2244=ADVANCED_FACE('',(#430,#257),#323,.T.);
#2245=ADVANCED_FACE('',(#431),#324,.T.);
#2246=ADVANCED_FACE('',(#432,#258),#325,.T.);
#2247=ADVANCED_FACE('',(#433),#2138,.T.);
#2248=ADVANCED_FACE('',(#434,#259),#326,.T.);
#2249=ADVANCED_FACE('',(#435),#2139,.F.);
#2250=ADVANCED_FACE('',(#436,#260),#327,.T.);
#2251=ADVANCED_FACE('',(#437),#2140,.T.);
#2252=ADVANCED_FACE('',(#438,#261),#328,.T.);
#2253=ADVANCED_FACE('',(#439),#2141,.F.);
#2254=ADVANCED_FACE('',(#440),#2142,.F.);
#2255=ADVANCED_FACE('',(#441),#2143,.T.);
#2256=ADVANCED_FACE('',(#442,#262),#329,.T.);
#2257=ADVANCED_FACE('',(#443,#263),#330,.F.);
#2258=ADVANCED_FACE('',(#444),#2144,.F.);
#2259=ADVANCED_FACE('',(#445),#2145,.F.);
#2260=ADVANCED_FACE('',(#446),#2146,.F.);
#2261=ADVANCED_FACE('',(#447),#2147,.F.);
#2262=ADVANCED_FACE('',(#448),#2148,.T.);
#2263=ADVANCED_FACE('',(#449,#264),#331,.T.);
#2264=ADVANCED_FACE('',(#450),#2149,.F.);
#2265=ADVANCED_FACE('',(#451,#265),#332,.F.);
#2266=ADVANCED_FACE('',(#452),#2150,.F.);
#2267=ADVANCED_FACE('',(#453),#2151,.T.);
#2268=ADVANCED_FACE('',(#454,#266,#267,#268,#269,#270),#333,.T.);
#2269=ADVANCED_FACE('',(#455,#271,#272,#273,#274,#275),#334,.F.);
#2270=ADVANCED_FACE('',(#456),#2152,.F.);
#2271=ADVANCED_FACE('',(#457),#2153,.T.);
#2272=ADVANCED_FACE('',(#458,#276),#335,.T.);
#2273=ADVANCED_FACE('',(#459,#277),#336,.F.);
#2274=ADVANCED_FACE('',(#460),#2154,.F.);
#2275=ADVANCED_FACE('',(#461),#2155,.F.);
#2276=ADVANCED_FACE('',(#462),#2156,.F.);
#2277=ADVANCED_FACE('',(#463),#2157,.F.);
#2278=ADVANCED_FACE('',(#464),#2158,.T.);
#2279=ADVANCED_FACE('',(#465,#278),#337,.F.);
#2280=ADVANCED_FACE('',(#466),#2159,.F.);
#2281=ADVANCED_FACE('',(#467),#2160,.T.);
#2282=ADVANCED_FACE('',(#468,#279,#280,#281,#282,#283),#338,.T.);
#2283=ADVANCED_FACE('',(#469,#284,#285,#286,#287,#288),#339,.F.);
#2284=ADVANCED_FACE('',(#470),#340,.T.);
#2285=ADVANCED_FACE('',(#471),#156,.T.);
#2286=ADVANCED_FACE('',(#472),#2161,.T.);
#2287=ADVANCED_FACE('',(#473),#157,.T.);
#2288=ADVANCED_FACE('',(#474,#289),#341,.T.);
#2289=ADVANCED_FACE('',(#475),#158,.T.);
#2290=ADVANCED_FACE('',(#476),#2162,.T.);
#2291=ADVANCED_FACE('',(#477),#159,.T.);
#2292=ADVANCED_FACE('',(#478),#342,.T.);
#2293=ADVANCED_FACE('',(#479),#343,.F.);
#2294=ADVANCED_FACE('',(#480),#344,.F.);
#2295=ADVANCED_FACE('',(#481),#345,.F.);
#2296=ADVANCED_FACE('',(#482),#346,.F.);
#2297=ADVANCED_FACE('',(#483),#347,.F.);
#2298=ADVANCED_FACE('',(#484),#348,.F.);
#2299=ADVANCED_FACE('',(#485),#349,.F.);
#2300=ADVANCED_FACE('',(#486),#350,.F.);
#2301=ADVANCED_FACE('',(#487),#2163,.T.);
#2302=ADVANCED_FACE('',(#488,#290),#351,.F.);
#2303=ADVANCED_FACE('',(#489,#291),#352,.T.);
#2304=ADVANCED_FACE('',(#490),#2164,.T.);
#2305=ADVANCED_FACE('',(#491,#292),#353,.T.);
#2306=ADVANCED_FACE('',(#492,#293),#354,.F.);
#2307=ADVANCED_FACE('',(#493),#2165,.T.);
#2308=ADVANCED_FACE('',(#494),#2166,.T.);
#2309=ADVANCED_FACE('',(#495),#2167,.T.);
#2310=ADVANCED_FACE('',(#496),#355,.T.);
#2311=ADVANCED_FACE('',(#497),#356,.F.);
#2312=ADVANCED_FACE('',(#498),#2168,.F.);
#2313=ADVANCED_FACE('',(#499),#2169,.T.);
#2314=ADVANCED_FACE('',(#500,#294),#357,.T.);
#2315=ADVANCED_FACE('',(#501,#295),#358,.F.);
#2316=ADVANCED_FACE('',(#502),#2170,.F.);
#2317=ADVANCED_FACE('',(#503),#2171,.T.);
#2318=ADVANCED_FACE('',(#504,#296,#297),#359,.F.);
#2319=ADVANCED_FACE('',(#505),#2172,.F.);
#2320=ADVANCED_FACE('',(#506),#2173,.F.);
#2321=ADVANCED_FACE('',(#507),#2174,.T.);
#2322=ADVANCED_FACE('',(#508),#11,.T.);
#2323=ADVANCED_FACE('',(#509,#298,#299),#360,.T.);
#2324=CLOSED_SHELL('',(#2175,#2176,#2177,#2178,#2179,#2180,#2181,#2182,
#2183,#2184,#2185,#2186,#2187,#2188,#2189,#2190,#2191,#2192,#2193,#2194,
#2195,#2196,#2197,#2198,#2199,#2200,#2201,#2202));
#2325=CLOSED_SHELL('',(#2203,#2204,#2205,#2206,#2207,#2208,#2209,#2210));
#2326=CLOSED_SHELL('',(#2211,#2212,#2213,#2214,#2215,#2216,#2217,#2218));
#2327=CLOSED_SHELL('',(#2219));
#2328=CLOSED_SHELL('',(#2220));
#2329=CLOSED_SHELL('',(#2221));
#2330=CLOSED_SHELL('',(#2222));
#2331=CLOSED_SHELL('',(#2223));
#2332=CLOSED_SHELL('',(#2224));
#2333=CLOSED_SHELL('',(#2225));
#2334=CLOSED_SHELL('',(#2226));
#2335=CLOSED_SHELL('',(#2227,#2228,#2229,#2230,#2231,#2232,#2233,#2234,
#2235,#2236,#2237,#2238,#2239,#2240,#2241,#2242,#2243,#2244,#2245));
#2336=CLOSED_SHELL('',(#2246,#2247,#2248,#2249));
#2337=CLOSED_SHELL('',(#2250,#2251,#2252,#2253));
#2338=CLOSED_SHELL('',(#2254,#2255,#2256,#2257));
#2339=CLOSED_SHELL('',(#2258,#2259,#2260,#2261,#2262,#2263,#2264,#2265,
#2266,#2267,#2268,#2269));
#2340=CLOSED_SHELL('',(#2270,#2271,#2272,#2273));
#2341=CLOSED_SHELL('',(#2274,#2275,#2276,#2277,#2278,#2279,#2280,#2281,
#2282,#2283));
#2342=CLOSED_SHELL('',(#2284,#2285,#2286,#2287,#2288,#2289,#2290,#2291,
#2292));
#2343=CLOSED_SHELL('',(#2293,#2294,#2295,#2296,#2297,#2298,#2299,#2300));
#2344=CLOSED_SHELL('',(#2301,#2302,#2303,#2304,#2305,#2306,#2307,#2308,
#2309,#2310,#2311));
#2345=CLOSED_SHELL('',(#2312,#2313,#2314,#2315));
#2346=CLOSED_SHELL('',(#2316,#2317,#2318,#2319,#2320,#2321,#2322,#2323));
#2347=DERIVED_UNIT_ELEMENT(#2375,1.);
#2348=DERIVED_UNIT_ELEMENT(#5537,-3.);
#2349=DERIVED_UNIT_ELEMENT(#2375,1.);
#2350=DERIVED_UNIT_ELEMENT(#5537,-3.);
#2351=DERIVED_UNIT_ELEMENT(#2375,1.);
#2352=DERIVED_UNIT_ELEMENT(#5537,-3.);
#2353=DERIVED_UNIT_ELEMENT(#2375,1.);
#2354=DERIVED_UNIT_ELEMENT(#5537,-3.);
#2355=DERIVED_UNIT_ELEMENT(#2375,1.);
#2356=DERIVED_UNIT_ELEMENT(#5537,-3.);
#2357=DERIVED_UNIT_ELEMENT(#2375,1.);
#2358=DERIVED_UNIT_ELEMENT(#5537,-3.);
#2359=DERIVED_UNIT_ELEMENT(#2375,1.);
#2360=DERIVED_UNIT_ELEMENT(#5537,-3.);
#2361=DERIVED_UNIT_ELEMENT(#2375,1.);
#2362=DERIVED_UNIT_ELEMENT(#5537,-3.);
#2363=DERIVED_UNIT_ELEMENT(#2375,1.);
#2364=DERIVED_UNIT_ELEMENT(#5537,-3.);
#2365=DERIVED_UNIT_ELEMENT(#2375,1.);
#2366=DERIVED_UNIT_ELEMENT(#5537,-3.);
#2367=DERIVED_UNIT_ELEMENT(#2375,1.);
#2368=DERIVED_UNIT_ELEMENT(#5537,-3.);
#2369=DERIVED_UNIT_ELEMENT(#2375,1.);
#2370=DERIVED_UNIT_ELEMENT(#5537,-3.);
#2371=DERIVED_UNIT_ELEMENT(#2375,1.);
#2372=DERIVED_UNIT_ELEMENT(#5537,-3.);
#2373=DERIVED_UNIT_ELEMENT(#2375,1.);
#2374=DERIVED_UNIT_ELEMENT(#5537,-3.);
#2375=(
MASS_UNIT()
NAMED_UNIT(*)
SI_UNIT(.KILO.,.GRAM.)
);
#2376=DERIVED_UNIT((#2347,#2348));
#2377=DERIVED_UNIT((#2349,#2350));
#2378=DERIVED_UNIT((#2351,#2352));
#2379=DERIVED_UNIT((#2353,#2354));
#2380=DERIVED_UNIT((#2355,#2356));
#2381=DERIVED_UNIT((#2357,#2358));
#2382=DERIVED_UNIT((#2359,#2360));
#2383=DERIVED_UNIT((#2361,#2362));
#2384=DERIVED_UNIT((#2363,#2364));
#2385=DERIVED_UNIT((#2365,#2366));
#2386=DERIVED_UNIT((#2367,#2368));
#2387=DERIVED_UNIT((#2369,#2370));
#2388=DERIVED_UNIT((#2371,#2372));
#2389=DERIVED_UNIT((#2373,#2374));
#2390=MEASURE_REPRESENTATION_ITEM('density measure',
POSITIVE_RATIO_MEASURE(7850.),#2376);
#2391=MEASURE_REPRESENTATION_ITEM('density measure',
POSITIVE_RATIO_MEASURE(7850.),#2377);
#2392=MEASURE_REPRESENTATION_ITEM('density measure',
POSITIVE_RATIO_MEASURE(7850.),#2378);
#2393=MEASURE_REPRESENTATION_ITEM('density measure',
POSITIVE_RATIO_MEASURE(7850.),#2379);
#2394=MEASURE_REPRESENTATION_ITEM('density measure',
POSITIVE_RATIO_MEASURE(7850.),#2380);
#2395=MEASURE_REPRESENTATION_ITEM('density measure',
POSITIVE_RATIO_MEASURE(7850.),#2381);
#2396=MEASURE_REPRESENTATION_ITEM('density measure',
POSITIVE_RATIO_MEASURE(7850.),#2382);
#2397=MEASURE_REPRESENTATION_ITEM('density measure',
POSITIVE_RATIO_MEASURE(7850.),#2383);
#2398=MEASURE_REPRESENTATION_ITEM('density measure',
POSITIVE_RATIO_MEASURE(7850.),#2384);
#2399=MEASURE_REPRESENTATION_ITEM('density measure',
POSITIVE_RATIO_MEASURE(7850.),#2385);
#2400=MEASURE_REPRESENTATION_ITEM('density measure',
POSITIVE_RATIO_MEASURE(7850.),#2386);
#2401=MEASURE_REPRESENTATION_ITEM('density measure',
POSITIVE_RATIO_MEASURE(7850.),#2387);
#2402=MEASURE_REPRESENTATION_ITEM('density measure',
POSITIVE_RATIO_MEASURE(7850.),#2388);
#2403=MEASURE_REPRESENTATION_ITEM('density measure',
POSITIVE_RATIO_MEASURE(7850.),#2389);
#2404=PROPERTY_DEFINITION_REPRESENTATION(#2474,#2432);
#2405=PROPERTY_DEFINITION_REPRESENTATION(#2475,#2433);
#2406=PROPERTY_DEFINITION_REPRESENTATION(#2476,#2434);
#2407=PROPERTY_DEFINITION_REPRESENTATION(#2477,#2435);
#2408=PROPERTY_DEFINITION_REPRESENTATION(#2478,#2436);
#2409=PROPERTY_DEFINITION_REPRESENTATION(#2479,#2437);
#2410=PROPERTY_DEFINITION_REPRESENTATION(#2480,#2438);
#2411=PROPERTY_DEFINITION_REPRESENTATION(#2481,#2439);
#2412=PROPERTY_DEFINITION_REPRESENTATION(#2482,#2440);
#2413=PROPERTY_DEFINITION_REPRESENTATION(#2483,#2441);
#2414=PROPERTY_DEFINITION_REPRESENTATION(#2484,#2442);
#2415=PROPERTY_DEFINITION_REPRESENTATION(#2485,#2443);
#2416=PROPERTY_DEFINITION_REPRESENTATION(#2486,#2444);
#2417=PROPERTY_DEFINITION_REPRESENTATION(#2487,#2445);
#2418=PROPERTY_DEFINITION_REPRESENTATION(#2488,#2446);
#2419=PROPERTY_DEFINITION_REPRESENTATION(#2489,#2447);
#2420=PROPERTY_DEFINITION_REPRESENTATION(#2490,#2448);
#2421=PROPERTY_DEFINITION_REPRESENTATION(#2491,#2449);
#2422=PROPERTY_DEFINITION_REPRESENTATION(#2492,#2450);
#2423=PROPERTY_DEFINITION_REPRESENTATION(#2493,#2451);
#2424=PROPERTY_DEFINITION_REPRESENTATION(#2494,#2452);
#2425=PROPERTY_DEFINITION_REPRESENTATION(#2495,#2453);
#2426=PROPERTY_DEFINITION_REPRESENTATION(#2496,#2454);
#2427=PROPERTY_DEFINITION_REPRESENTATION(#2497,#2455);
#2428=PROPERTY_DEFINITION_REPRESENTATION(#2498,#2456);
#2429=PROPERTY_DEFINITION_REPRESENTATION(#2499,#2457);
#2430=PROPERTY_DEFINITION_REPRESENTATION(#2500,#2458);
#2431=PROPERTY_DEFINITION_REPRESENTATION(#2501,#2459);
#2432=REPRESENTATION('material name',(#2460),#5519);
#2433=REPRESENTATION('density',(#2390),#5519);
#2434=REPRESENTATION('material name',(#2461),#5521);
#2435=REPRESENTATION('density',(#2391),#5521);
#2436=REPRESENTATION('material name',(#2462),#5522);
#2437=REPRESENTATION('density',(#2392),#5522);
#2438=REPRESENTATION('material name',(#2463),#5523);
#2439=REPRESENTATION('density',(#2393),#5523);
#2440=REPRESENTATION('material name',(#2464),#5524);
#2441=REPRESENTATION('density',(#2394),#5524);
#2442=REPRESENTATION('material name',(#2465),#5525);
#2443=REPRESENTATION('density',(#2395),#5525);
#2444=REPRESENTATION('material name',(#2466),#5526);
#2445=REPRESENTATION('density',(#2396),#5526);
#2446=REPRESENTATION('material name',(#2467),#5527);
#2447=REPRESENTATION('density',(#2397),#5527);
#2448=REPRESENTATION('material name',(#2468),#5528);
#2449=REPRESENTATION('density',(#2398),#5528);
#2450=REPRESENTATION('material name',(#2469),#5529);
#2451=REPRESENTATION('density',(#2399),#5529);
#2452=REPRESENTATION('material name',(#2470),#5530);
#2453=REPRESENTATION('density',(#2400),#5530);
#2454=REPRESENTATION('material name',(#2471),#5532);
#2455=REPRESENTATION('density',(#2401),#5532);
#2456=REPRESENTATION('material name',(#2472),#5533);
#2457=REPRESENTATION('density',(#2402),#5533);
#2458=REPRESENTATION('material name',(#2473),#5534);
#2459=REPRESENTATION('density',(#2403),#5534);
#2460=DESCRIPTIVE_REPRESENTATION_ITEM('Steel','Steel');
#2461=DESCRIPTIVE_REPRESENTATION_ITEM('Steel','Steel');
#2462=DESCRIPTIVE_REPRESENTATION_ITEM('Steel','Steel');
#2463=DESCRIPTIVE_REPRESENTATION_ITEM('Steel','Steel');
#2464=DESCRIPTIVE_REPRESENTATION_ITEM('Steel','Steel');
#2465=DESCRIPTIVE_REPRESENTATION_ITEM('Steel','Steel');
#2466=DESCRIPTIVE_REPRESENTATION_ITEM('Steel','Steel');
#2467=DESCRIPTIVE_REPRESENTATION_ITEM('Steel','Steel');
#2468=DESCRIPTIVE_REPRESENTATION_ITEM('Steel','Steel');
#2469=DESCRIPTIVE_REPRESENTATION_ITEM('Steel','Steel');
#2470=DESCRIPTIVE_REPRESENTATION_ITEM('Steel','Steel');
#2471=DESCRIPTIVE_REPRESENTATION_ITEM('Steel','Steel');
#2472=DESCRIPTIVE_REPRESENTATION_ITEM('Steel','Steel');
#2473=DESCRIPTIVE_REPRESENTATION_ITEM('Steel','Steel');
#2474=PROPERTY_DEFINITION('material property','material name',#5622);
#2475=PROPERTY_DEFINITION('material property','density of part',#5622);
#2476=PROPERTY_DEFINITION('material property','material name',#5624);
#2477=PROPERTY_DEFINITION('material property','density of part',#5624);
#2478=PROPERTY_DEFINITION('material property','material name',#5625);
#2479=PROPERTY_DEFINITION('material property','density of part',#5625);
#2480=PROPERTY_DEFINITION('material property','material name',#5626);
#2481=PROPERTY_DEFINITION('material property','density of part',#5626);
#2482=PROPERTY_DEFINITION('material property','material name',#5627);
#2483=PROPERTY_DEFINITION('material property','density of part',#5627);
#2484=PROPERTY_DEFINITION('material property','material name',#5628);
#2485=PROPERTY_DEFINITION('material property','density of part',#5628);
#2486=PROPERTY_DEFINITION('material property','material name',#5629);
#2487=PROPERTY_DEFINITION('material property','density of part',#5629);
#2488=PROPERTY_DEFINITION('material property','material name',#5630);
#2489=PROPERTY_DEFINITION('material property','density of part',#5630);
#2490=PROPERTY_DEFINITION('material property','material name',#5631);
#2491=PROPERTY_DEFINITION('material property','density of part',#5631);
#2492=PROPERTY_DEFINITION('material property','material name',#5632);
#2493=PROPERTY_DEFINITION('material property','density of part',#5632);
#2494=PROPERTY_DEFINITION('material property','material name',#5633);
#2495=PROPERTY_DEFINITION('material property','density of part',#5633);
#2496=PROPERTY_DEFINITION('material property','material name',#5635);
#2497=PROPERTY_DEFINITION('material property','density of part',#5635);
#2498=PROPERTY_DEFINITION('material property','material name',#5636);
#2499=PROPERTY_DEFINITION('material property','density of part',#5636);
#2500=PROPERTY_DEFINITION('material property','material name',#5637);
#2501=PROPERTY_DEFINITION('material property','density of part',#5637);
#2502=AXIS2_PLACEMENT_3D('',#3683,#2867,#2868);
#2503=AXIS2_PLACEMENT_3D('',#3684,#2869,#2870);
#2504=AXIS2_PLACEMENT_3D('',#3685,#2871,#2872);
#2505=AXIS2_PLACEMENT_3D('',#3686,#2873,#2874);
#2506=AXIS2_PLACEMENT_3D('',#3688,#2875,#2876);
#2507=AXIS2_PLACEMENT_3D('',#3691,#2878,#2879);
#2508=AXIS2_PLACEMENT_3D('',#3692,#2880,#2881);
#2509=AXIS2_PLACEMENT_3D('',#3694,#2882,#2883);
#2510=AXIS2_PLACEMENT_3D('',#3697,#2885,#2886);
#2511=AXIS2_PLACEMENT_3D('',#3698,#2887,#2888);
#2512=AXIS2_PLACEMENT_3D('',#3700,#2889,#2890);
#2513=AXIS2_PLACEMENT_3D('',#3703,#2892,#2893);
#2514=AXIS2_PLACEMENT_3D('',#3704,#2894,#2895);
#2515=AXIS2_PLACEMENT_3D('',#3706,#2896,#2897);
#2516=AXIS2_PLACEMENT_3D('',#3709,#2899,#2900);
#2517=AXIS2_PLACEMENT_3D('',#3710,#2901,#2902);
#2518=AXIS2_PLACEMENT_3D('',#3712,#2903,#2904);
#2519=AXIS2_PLACEMENT_3D('',#3715,#2906,#2907);
#2520=AXIS2_PLACEMENT_3D('',#3716,#2908,#2909);
#2521=AXIS2_PLACEMENT_3D('',#3717,#2910,#2911);
#2522=AXIS2_PLACEMENT_3D('',#3719,#2912,#2913);
#2523=AXIS2_PLACEMENT_3D('',#3722,#2915,#2916);
#2524=AXIS2_PLACEMENT_3D('',#3723,#2917,#2918);
#2525=AXIS2_PLACEMENT_3D('',#3724,#2919,#2920);
#2526=AXIS2_PLACEMENT_3D('',#3726,#2921,#2922);
#2527=AXIS2_PLACEMENT_3D('',#3729,#2924,#2925);
#2528=AXIS2_PLACEMENT_3D('',#3730,#2926,#2927);
#2529=AXIS2_PLACEMENT_3D('',#3731,#2928,#2929);
#2530=AXIS2_PLACEMENT_3D('',#3733,#2930,#2931);
#2531=AXIS2_PLACEMENT_3D('',#3736,#2933,#2934);
#2532=AXIS2_PLACEMENT_3D('',#3737,#2935,#2936);
#2533=AXIS2_PLACEMENT_3D('',#3738,#2937,#2938);
#2534=AXIS2_PLACEMENT_3D('',#3740,#2939,#2940);
#2535=AXIS2_PLACEMENT_3D('',#3743,#2942,#2943);
#2536=AXIS2_PLACEMENT_3D('',#3744,#2944,#2945);
#2537=AXIS2_PLACEMENT_3D('',#3745,#2946,#2947);
#2538=AXIS2_PLACEMENT_3D('',#3747,#2948,#2949);
#2539=AXIS2_PLACEMENT_3D('',#3750,#2951,#2952);
#2540=AXIS2_PLACEMENT_3D('',#3751,#2953,#2954);
#2541=AXIS2_PLACEMENT_3D('',#3752,#2955,#2956);
#2542=AXIS2_PLACEMENT_3D('',#3754,#2957,#2958);
#2543=AXIS2_PLACEMENT_3D('',#3757,#2960,#2961);
#2544=AXIS2_PLACEMENT_3D('',#3758,#2962,#2963);
#2545=AXIS2_PLACEMENT_3D('',#3759,#2964,#2965);
#2546=AXIS2_PLACEMENT_3D('',#3761,#2966,#2967);
#2547=AXIS2_PLACEMENT_3D('',#3764,#2969,#2970);
#2548=AXIS2_PLACEMENT_3D('',#3765,#2971,#2972);
#2549=AXIS2_PLACEMENT_3D('',#3766,#2973,#2974);
#2550=AXIS2_PLACEMENT_3D('',#3768,#2975,#2976);
#2551=AXIS2_PLACEMENT_3D('',#3770,#2977,#2978);
#2552=AXIS2_PLACEMENT_3D('',#3771,#2979,#2980);
#2553=AXIS2_PLACEMENT_3D('',#3773,#2981,#2982);
#2554=AXIS2_PLACEMENT_3D('',#3775,#2983,#2984);
#2555=AXIS2_PLACEMENT_3D('',#3776,#2985,#2986);
#2556=AXIS2_PLACEMENT_3D('',#3778,#2988,#2989);
#2557=AXIS2_PLACEMENT_3D('',#3781,#2991,#2992);
#2558=AXIS2_PLACEMENT_3D('',#3782,#2993,#2994);
#2559=AXIS2_PLACEMENT_3D('',#3784,#2995,#2996);
#2560=AXIS2_PLACEMENT_3D('',#3787,#2998,#2999);
#2561=AXIS2_PLACEMENT_3D('',#3788,#3000,#3001);
#2562=AXIS2_PLACEMENT_3D('',#3790,#3002,#3003);
#2563=AXIS2_PLACEMENT_3D('',#3792,#3005,#3006);
#2564=AXIS2_PLACEMENT_3D('',#3793,#3007,#3008);
#2565=AXIS2_PLACEMENT_3D('',#3794,#3009,#3010);
#2566=AXIS2_PLACEMENT_3D('',#3795,#3011,#3012);
#2567=AXIS2_PLACEMENT_3D('',#3796,#3013,#3014);
#2568=AXIS2_PLACEMENT_3D('',#3799,#3015,#3016);
#2569=AXIS2_PLACEMENT_3D('',#3800,#3017,#3018);
#2570=AXIS2_PLACEMENT_3D('',#3802,#3019,#3020);
#2571=AXIS2_PLACEMENT_3D('',#3804,#3021,#3022);
#2572=AXIS2_PLACEMENT_3D('',#3805,#3023,#3024);
#2573=AXIS2_PLACEMENT_3D('',#3806,#3025,#3026);
#2574=AXIS2_PLACEMENT_3D('',#3809,#3028,#3029);
#2575=AXIS2_PLACEMENT_3D('',#3810,#3030,#3031);
#2576=AXIS2_PLACEMENT_3D('',#3812,#3032,#3033);
#2577=AXIS2_PLACEMENT_3D('',#3815,#3035,#3036);
#2578=AXIS2_PLACEMENT_3D('',#3816,#3037,#3038);
#2579=AXIS2_PLACEMENT_3D('',#3819,#3040,#3041);
#2580=AXIS2_PLACEMENT_3D('',#3820,#3042,#3043);
#2581=AXIS2_PLACEMENT_3D('',#3821,#3044,#3045);
#2582=AXIS2_PLACEMENT_3D('',#3823,#3046,#3047);
#2583=AXIS2_PLACEMENT_3D('',#3825,#3049,#3050);
#2584=AXIS2_PLACEMENT_3D('',#3827,#3051,#3052);
#2585=AXIS2_PLACEMENT_3D('',#3828,#3053,#3054);
#2586=AXIS2_PLACEMENT_3D('',#3830,#3056,#3057);
#2587=AXIS2_PLACEMENT_3D('',#3831,#3058,#3059);
#2588=AXIS2_PLACEMENT_3D('',#3834,#3060,#3061);
#2589=AXIS2_PLACEMENT_3D('',#3835,#3062,#3063);
#2590=AXIS2_PLACEMENT_3D('',#3837,#3064,#3065);
#2591=AXIS2_PLACEMENT_3D('',#3839,#3066,#3067);
#2592=AXIS2_PLACEMENT_3D('',#3840,#3068,#3069);
#2593=AXIS2_PLACEMENT_3D('',#3841,#3070,#3071);
#2594=AXIS2_PLACEMENT_3D('',#3843,#3072,#3073);
#2595=AXIS2_PLACEMENT_3D('',#3845,#3075,#3076);
#2596=AXIS2_PLACEMENT_3D('',#3847,#3077,#3078);
#2597=AXIS2_PLACEMENT_3D('',#3849,#3079,#3080);
#2598=AXIS2_PLACEMENT_3D('',#3850,#3081,#3082);
#2599=AXIS2_PLACEMENT_3D('',#3852,#3083,#3084);
#2600=AXIS2_PLACEMENT_3D('',#3854,#3086,#3087);
#2601=AXIS2_PLACEMENT_3D('',#3856,#3088,#3089);
#2602=AXIS2_PLACEMENT_3D('',#3858,#3091,#3092);
#2603=AXIS2_PLACEMENT_3D('',#3860,#3093,#3094);
#2604=AXIS2_PLACEMENT_3D('',#3862,#3096,#3097);
#2605=AXIS2_PLACEMENT_3D('',#3863,#3098,#3099);
#2606=AXIS2_PLACEMENT_3D('',#3865,#3101,#3102);
#2607=AXIS2_PLACEMENT_3D('',#3866,#3103,#3104);
#2608=AXIS2_PLACEMENT_3D('',#3869,#3105,#3106);
#2609=AXIS2_PLACEMENT_3D('',#3870,#3107,#3108);
#2610=AXIS2_PLACEMENT_3D('',#3873,#3109,#3110);
#2611=AXIS2_PLACEMENT_3D('',#3874,#3111,#3112);
#2612=AXIS2_PLACEMENT_3D('',#3877,#3113,#3114);
#2613=AXIS2_PLACEMENT_3D('',#3878,#3115,#3116);
#2614=AXIS2_PLACEMENT_3D('',#3881,#3117,#3118);
#2615=AXIS2_PLACEMENT_3D('',#3882,#3119,#3120);
#2616=AXIS2_PLACEMENT_3D('',#3885,#3121,#3122);
#2617=AXIS2_PLACEMENT_3D('',#3886,#3123,#3124);
#2618=AXIS2_PLACEMENT_3D('',#3889,#3125,#3126);
#2619=AXIS2_PLACEMENT_3D('',#3890,#3127,#3128);
#2620=AXIS2_PLACEMENT_3D('',#3893,#3129,#3130);
#2621=AXIS2_PLACEMENT_3D('',#3894,#3131,#3132);
#2622=AXIS2_PLACEMENT_3D('',#3897,#3133,#3134);
#2623=AXIS2_PLACEMENT_3D('',#3898,#3135,#3136);
#2624=AXIS2_PLACEMENT_3D('',#3899,#3137,#3138);
#2625=AXIS2_PLACEMENT_3D('',#3925,#3139,#3140);
#2626=AXIS2_PLACEMENT_3D('',#3949,#3141,#3142);
#2627=AXIS2_PLACEMENT_3D('',#3950,#3143,#3144);
#2628=AXIS2_PLACEMENT_3D('',#3952,#3145,#3146);
#2629=AXIS2_PLACEMENT_3D('',#3977,#3147,#3148);
#2630=AXIS2_PLACEMENT_3D('',#4002,#3149,#3150);
#2631=AXIS2_PLACEMENT_3D('',#4018,#3152,#3153);
#2632=AXIS2_PLACEMENT_3D('',#4033,#3154,#3155);
#2633=AXIS2_PLACEMENT_3D('',#4058,#3156,#3157);
#2634=AXIS2_PLACEMENT_3D('',#4083,#3158,#3159);
#2635=AXIS2_PLACEMENT_3D('',#4108,#3160,#3161);
#2636=AXIS2_PLACEMENT_3D('',#4132,#3162,#3163);
#2637=AXIS2_PLACEMENT_3D('',#4133,#3164,#3165);
#2638=AXIS2_PLACEMENT_3D('',#4135,#3166,#3167);
#2639=AXIS2_PLACEMENT_3D('',#4136,#3168,#3169);
#2640=AXIS2_PLACEMENT_3D('',#4137,#3170,#3171);
#2641=AXIS2_PLACEMENT_3D('',#4161,#3172,#3173);
#2642=AXIS2_PLACEMENT_3D('',#4162,#3174,#3175);
#2643=AXIS2_PLACEMENT_3D('',#4164,#3176,#3177);
#2644=AXIS2_PLACEMENT_3D('',#4165,#3178,#3179);
#2645=AXIS2_PLACEMENT_3D('',#4166,#3180,#3181);
#2646=AXIS2_PLACEMENT_3D('',#4190,#3182,#3183);
#2647=AXIS2_PLACEMENT_3D('',#4191,#3184,#3185);
#2648=AXIS2_PLACEMENT_3D('',#4193,#3186,#3187);
#2649=AXIS2_PLACEMENT_3D('',#4194,#3188,#3189);
#2650=AXIS2_PLACEMENT_3D('',#4195,#3190,#3191);
#2651=AXIS2_PLACEMENT_3D('',#4210,#3192,#3193);
#2652=AXIS2_PLACEMENT_3D('',#4223,#3194,#3195);
#2653=AXIS2_PLACEMENT_3D('',#4225,#3196,#3197);
#2654=AXIS2_PLACEMENT_3D('',#4226,#3198,#3199);
#2655=AXIS2_PLACEMENT_3D('',#4227,#3200,#3201);
#2656=AXIS2_PLACEMENT_3D('',#4251,#3202,#3203);
#2657=AXIS2_PLACEMENT_3D('',#4252,#3204,#3205);
#2658=AXIS2_PLACEMENT_3D('',#4254,#3206,#3207);
#2659=AXIS2_PLACEMENT_3D('',#4255,#3208,#3209);
#2660=AXIS2_PLACEMENT_3D('',#4256,#3210,#3211);
#2661=AXIS2_PLACEMENT_3D('',#4280,#3212,#3213);
#2662=AXIS2_PLACEMENT_3D('',#4281,#3214,#3215);
#2663=AXIS2_PLACEMENT_3D('',#4283,#3216,#3217);
#2664=AXIS2_PLACEMENT_3D('',#4284,#3218,#3219);
#2665=AXIS2_PLACEMENT_3D('',#4285,#3220,#3221);
#2666=AXIS2_PLACEMENT_3D('',#4309,#3222,#3223);
#2667=AXIS2_PLACEMENT_3D('',#4310,#3224,#3225);
#2668=AXIS2_PLACEMENT_3D('',#4312,#3226,#3227);
#2669=AXIS2_PLACEMENT_3D('',#4315,#3229,#3230);
#2670=AXIS2_PLACEMENT_3D('',#4339,#3231,#3232);
#2671=AXIS2_PLACEMENT_3D('',#4340,#3233,#3234);
#2672=AXIS2_PLACEMENT_3D('',#4341,#3235,#3236);
#2673=AXIS2_PLACEMENT_3D('',#4342,#3237,#3238);
#2674=AXIS2_PLACEMENT_3D('',#4343,#3239,#3240);
#2675=AXIS2_PLACEMENT_3D('',#4344,#3241,#3242);
#2676=AXIS2_PLACEMENT_3D('',#4345,#3243,#3244);
#2677=AXIS2_PLACEMENT_3D('',#4346,#3245,#3246);
#2678=AXIS2_PLACEMENT_3D('',#4347,#3247,#3248);
#2679=AXIS2_PLACEMENT_3D('',#4349,#3249,#3250);
#2680=AXIS2_PLACEMENT_3D('',#4351,#3251,#3252);
#2681=AXIS2_PLACEMENT_3D('',#4352,#3253,#3254);
#2682=AXIS2_PLACEMENT_3D('',#4354,#3255,#3256);
#2683=AXIS2_PLACEMENT_3D('',#4356,#3258,#3259);
#2684=AXIS2_PLACEMENT_3D('',#4358,#3260,#3261);
#2685=AXIS2_PLACEMENT_3D('',#4359,#3262,#3263);
#2686=AXIS2_PLACEMENT_3D('',#4361,#3265,#3266);
#2687=AXIS2_PLACEMENT_3D('',#4363,#3267,#3268);
#2688=AXIS2_PLACEMENT_3D('',#4365,#3269,#3270);
#2689=AXIS2_PLACEMENT_3D('',#4366,#3271,#3272);
#2690=AXIS2_PLACEMENT_3D('',#4368,#3273,#3274);
#2691=AXIS2_PLACEMENT_3D('',#4370,#3276,#3277);
#2692=AXIS2_PLACEMENT_3D('',#4372,#3278,#3279);
#2693=AXIS2_PLACEMENT_3D('',#4373,#3280,#3281);
#2694=AXIS2_PLACEMENT_3D('',#4375,#3283,#3284);
#2695=AXIS2_PLACEMENT_3D('',#4376,#3285,#3286);
#2696=AXIS2_PLACEMENT_3D('',#4377,#3287,#3288);
#2697=AXIS2_PLACEMENT_3D('',#4378,#3289,#3290);
#2698=AXIS2_PLACEMENT_3D('',#4379,#3291,#3292);
#2699=AXIS2_PLACEMENT_3D('',#4380,#3293,#3294);
#2700=AXIS2_PLACEMENT_3D('',#4381,#3295,#3296);
#2701=AXIS2_PLACEMENT_3D('',#4383,#3297,#3298);
#2702=AXIS2_PLACEMENT_3D('',#4386,#3300,#3301);
#2703=AXIS2_PLACEMENT_3D('',#4387,#3302,#3303);
#2704=AXIS2_PLACEMENT_3D('',#4389,#3304,#3305);
#2705=AXIS2_PLACEMENT_3D('',#4392,#3307,#3308);
#2706=AXIS2_PLACEMENT_3D('',#4393,#3309,#3310);
#2707=AXIS2_PLACEMENT_3D('',#4394,#3311,#3312);
#2708=AXIS2_PLACEMENT_3D('',#4395,#3313,#3314);
#2709=AXIS2_PLACEMENT_3D('',#4396,#3315,#3316);
#2710=AXIS2_PLACEMENT_3D('',#4398,#3317,#3318);
#2711=AXIS2_PLACEMENT_3D('',#4401,#3320,#3321);
#2712=AXIS2_PLACEMENT_3D('',#4402,#3322,#3323);
#2713=AXIS2_PLACEMENT_3D('',#4404,#3324,#3325);
#2714=AXIS2_PLACEMENT_3D('',#4407,#3327,#3328);
#2715=AXIS2_PLACEMENT_3D('',#4408,#3329,#3330);
#2716=AXIS2_PLACEMENT_3D('',#4410,#3331,#3332);
#2717=AXIS2_PLACEMENT_3D('',#4413,#3334,#3335);
#2718=AXIS2_PLACEMENT_3D('',#4414,#3336,#3337);
#2719=AXIS2_PLACEMENT_3D('',#4416,#3338,#3339);
#2720=AXIS2_PLACEMENT_3D('',#4419,#3341,#3342);
#2721=AXIS2_PLACEMENT_3D('',#4420,#3343,#3344);
#2722=AXIS2_PLACEMENT_3D('',#4422,#3345,#3346);
#2723=AXIS2_PLACEMENT_3D('',#4425,#3348,#3349);
#2724=AXIS2_PLACEMENT_3D('',#4426,#3350,#3351);
#2725=AXIS2_PLACEMENT_3D('',#4428,#3352,#3353);
#2726=AXIS2_PLACEMENT_3D('',#4429,#3354,#3355);
#2727=AXIS2_PLACEMENT_3D('',#4431,#3356,#3357);
#2728=AXIS2_PLACEMENT_3D('',#4434,#3359,#3360);
#2729=AXIS2_PLACEMENT_3D('',#4435,#3361,#3362);
#2730=AXIS2_PLACEMENT_3D('',#4437,#3363,#3364);
#2731=AXIS2_PLACEMENT_3D('',#4438,#3365,#3366);
#2732=AXIS2_PLACEMENT_3D('',#4440,#3368,#3369);
#2733=AXIS2_PLACEMENT_3D('',#4442,#3370,#3371);
#2734=AXIS2_PLACEMENT_3D('',#4445,#3373,#3374);
#2735=AXIS2_PLACEMENT_3D('',#4446,#3375,#3376);
#2736=AXIS2_PLACEMENT_3D('',#4447,#3377,#3378);
#2737=AXIS2_PLACEMENT_3D('',#4448,#3379,#3380);
#2738=AXIS2_PLACEMENT_3D('',#4449,#3381,#3382);
#2739=AXIS2_PLACEMENT_3D('',#4451,#3383,#3384);
#2740=AXIS2_PLACEMENT_3D('',#4454,#3386,#3387);
#2741=AXIS2_PLACEMENT_3D('',#4455,#3388,#3389);
#2742=AXIS2_PLACEMENT_3D('',#4457,#3390,#3391);
#2743=AXIS2_PLACEMENT_3D('',#4460,#3393,#3394);
#2744=AXIS2_PLACEMENT_3D('',#4461,#3395,#3396);
#2745=AXIS2_PLACEMENT_3D('',#4462,#3397,#3398);
#2746=AXIS2_PLACEMENT_3D('',#4463,#3399,#3400);
#2747=AXIS2_PLACEMENT_3D('',#4464,#3401,#3402);
#2748=AXIS2_PLACEMENT_3D('',#4466,#3403,#3404);
#2749=AXIS2_PLACEMENT_3D('',#4469,#3406,#3407);
#2750=AXIS2_PLACEMENT_3D('',#4470,#3408,#3409);
#2751=AXIS2_PLACEMENT_3D('',#4472,#3410,#3411);
#2752=AXIS2_PLACEMENT_3D('',#4475,#3413,#3414);
#2753=AXIS2_PLACEMENT_3D('',#4476,#3415,#3416);
#2754=AXIS2_PLACEMENT_3D('',#4478,#3417,#3418);
#2755=AXIS2_PLACEMENT_3D('',#4481,#3420,#3421);
#2756=AXIS2_PLACEMENT_3D('',#4482,#3422,#3423);
#2757=AXIS2_PLACEMENT_3D('',#4484,#3424,#3425);
#2758=AXIS2_PLACEMENT_3D('',#4487,#3427,#3428);
#2759=AXIS2_PLACEMENT_3D('',#4488,#3429,#3430);
#2760=AXIS2_PLACEMENT_3D('',#4490,#3431,#3432);
#2761=AXIS2_PLACEMENT_3D('',#4493,#3434,#3435);
#2762=AXIS2_PLACEMENT_3D('',#4494,#3436,#3437);
#2763=AXIS2_PLACEMENT_3D('',#4496,#3438,#3439);
#2764=AXIS2_PLACEMENT_3D('',#4497,#3440,#3441);
#2765=AXIS2_PLACEMENT_3D('',#4499,#3442,#3443);
#2766=AXIS2_PLACEMENT_3D('',#4501,#3445,#3446);
#2767=AXIS2_PLACEMENT_3D('',#4503,#3447,#3448);
#2768=AXIS2_PLACEMENT_3D('',#4506,#3450,#3451);
#2769=AXIS2_PLACEMENT_3D('',#4507,#3452,#3453);
#2770=AXIS2_PLACEMENT_3D('',#4508,#3454,#3455);
#2771=AXIS2_PLACEMENT_3D('',#4509,#3456,#3457);
#2772=AXIS2_PLACEMENT_3D('',#4510,#3458,#3459);
#2773=AXIS2_PLACEMENT_3D('',#4512,#3460,#3461);
#2774=AXIS2_PLACEMENT_3D('',#4513,#3462,#3463);
#2775=AXIS2_PLACEMENT_3D('',#4515,#3464,#3465);
#2776=AXIS2_PLACEMENT_3D('',#4517,#3467,#3468);
#2777=AXIS2_PLACEMENT_3D('',#4519,#3469,#3470);
#2778=AXIS2_PLACEMENT_3D('',#4521,#3472,#3473);
#2779=AXIS2_PLACEMENT_3D('',#4523,#3474,#3475);
#2780=AXIS2_PLACEMENT_3D('',#4525,#3477,#3478);
#2781=AXIS2_PLACEMENT_3D('',#4527,#3479,#3480);
#2782=AXIS2_PLACEMENT_3D('',#4528,#3481,#3482);
#2783=AXIS2_PLACEMENT_3D('',#4530,#3483,#3484);
#2784=AXIS2_PLACEMENT_3D('',#4532,#3486,#3487);
#2785=AXIS2_PLACEMENT_3D('',#4534,#3488,#3489);
#2786=AXIS2_PLACEMENT_3D('',#4536,#3491,#3492);
#2787=AXIS2_PLACEMENT_3D('',#4538,#3493,#3494);
#2788=AXIS2_PLACEMENT_3D('',#4540,#3496,#3497);
#2789=AXIS2_PLACEMENT_3D('',#4541,#3498,#3499);
#2790=AXIS2_PLACEMENT_3D('',#4550,#3504,#3505);
#2791=AXIS2_PLACEMENT_3D('',#4556,#3509,#3510);
#2792=AXIS2_PLACEMENT_3D('',#4562,#3514,#3515);
#2793=AXIS2_PLACEMENT_3D('',#4568,#3519,#3520);
#2794=AXIS2_PLACEMENT_3D('',#4574,#3524,#3525);
#2795=AXIS2_PLACEMENT_3D('',#4577,#3528,#3529);
#2796=AXIS2_PLACEMENT_3D('',#4578,#3530,#3531);
#2797=AXIS2_PLACEMENT_3D('',#4579,#3532,#3533);
#2798=AXIS2_PLACEMENT_3D('',#4580,#3534,#3535);
#2799=AXIS2_PLACEMENT_3D('',#4581,#3536,#3537);
#2800=AXIS2_PLACEMENT_3D('',#4582,#3538,#3539);
#2801=AXIS2_PLACEMENT_3D('',#4583,#3540,#3541);
#2802=AXIS2_PLACEMENT_3D('',#4584,#3542,#3543);
#2803=AXIS2_PLACEMENT_3D('',#4585,#3544,#3545);
#2804=AXIS2_PLACEMENT_3D('',#4586,#3546,#3547);
#2805=AXIS2_PLACEMENT_3D('',#4587,#3548,#3549);
#2806=AXIS2_PLACEMENT_3D('',#4588,#3550,#3551);
#2807=AXIS2_PLACEMENT_3D('',#4589,#3552,#3553);
#2808=AXIS2_PLACEMENT_3D('',#4590,#3554,#3555);
#2809=AXIS2_PLACEMENT_3D('',#4591,#3556,#3557);
#2810=AXIS2_PLACEMENT_3D('',#4592,#3558,#3559);
#2811=AXIS2_PLACEMENT_3D('',#4593,#3560,#3561);
#2812=AXIS2_PLACEMENT_3D('',#4594,#3562,#3563);
#2813=AXIS2_PLACEMENT_3D('',#4595,#3564,#3565);
#2814=AXIS2_PLACEMENT_3D('',#4596,#3566,#3567);
#2815=AXIS2_PLACEMENT_3D('',#4598,#3568,#3569);
#2816=AXIS2_PLACEMENT_3D('',#4601,#3571,#3572);
#2817=AXIS2_PLACEMENT_3D('',#4602,#3573,#3574);
#2818=AXIS2_PLACEMENT_3D('',#4604,#3575,#3576);
#2819=AXIS2_PLACEMENT_3D('',#4605,#3577,#3578);
#2820=AXIS2_PLACEMENT_3D('',#4607,#3579,#3580);
#2821=AXIS2_PLACEMENT_3D('',#4608,#3581,#3582);
#2822=AXIS2_PLACEMENT_3D('',#4611,#3584,#3585);
#2823=AXIS2_PLACEMENT_3D('',#4612,#3586,#3587);
#2824=AXIS2_PLACEMENT_3D('',#4614,#3588,#3589);
#2825=AXIS2_PLACEMENT_3D('',#4615,#3590,#3591);
#2826=AXIS2_PLACEMENT_3D('',#4617,#3592,#3593);
#2827=AXIS2_PLACEMENT_3D('',#4619,#3594,#3595);
#2828=AXIS2_PLACEMENT_3D('',#4620,#3596,#3597);
#2829=AXIS2_PLACEMENT_3D('',#4622,#3599,#3600);
#2830=AXIS2_PLACEMENT_3D('',#4625,#3602,#3603);
#2831=AXIS2_PLACEMENT_3D('',#4626,#3604,#3605);
#2832=AXIS2_PLACEMENT_3D('',#4628,#3606,#3607);
#2833=AXIS2_PLACEMENT_3D('',#4630,#3609,#3610);
#2834=AXIS2_PLACEMENT_3D('',#4631,#3611,#3612);
#2835=AXIS2_PLACEMENT_3D('',#4632,#3613,#3614);
#2836=AXIS2_PLACEMENT_3D('',#4633,#3615,#3616);
#2837=AXIS2_PLACEMENT_3D('',#4635,#3617,#3618);
#2838=AXIS2_PLACEMENT_3D('',#4638,#3620,#3621);
#2839=AXIS2_PLACEMENT_3D('',#4639,#3622,#3623);
#2840=AXIS2_PLACEMENT_3D('',#4641,#3624,#3625);
#2841=AXIS2_PLACEMENT_3D('',#4644,#3627,#3628);
#2842=AXIS2_PLACEMENT_3D('',#4645,#3629,#3630);
#2843=AXIS2_PLACEMENT_3D('',#4646,#3631,#3632);
#2844=AXIS2_PLACEMENT_3D('',#4647,#3633,#3634);
#2845=AXIS2_PLACEMENT_3D('',#4648,#3635,#3636);
#2846=AXIS2_PLACEMENT_3D('',#4653,#3638,#3639);
#2847=AXIS2_PLACEMENT_3D('',#4656,#3641,#3642);
#2848=AXIS2_PLACEMENT_3D('',#4657,#3643,#3644);
#2849=AXIS2_PLACEMENT_3D('',#4659,#3645,#3646);
#2850=AXIS2_PLACEMENT_3D('',#4667,#3647,#3648);
#2851=AXIS2_PLACEMENT_3D('',#4668,#3649,#3650);
#2852=AXIS2_PLACEMENT_3D('',#4670,#3651,#3652);
#2853=AXIS2_PLACEMENT_3D('',#4867,#3653,#3654);
#2854=AXIS2_PLACEMENT_3D('',#4869,#3655,#3656);
#2855=AXIS2_PLACEMENT_3D('',#4870,#3657,#3658);
#2856=AXIS2_PLACEMENT_3D('',#4873,#3660,#3661);
#2857=AXIS2_PLACEMENT_3D('',#4874,#3662,#3663);
#2858=AXIS2_PLACEMENT_3D('',#4877,#3665,#3666);
#2859=AXIS2_PLACEMENT_3D('',#4878,#3667,#3668);
#2860=AXIS2_PLACEMENT_3D('',#4880,#3669,#3670);
#2861=AXIS2_PLACEMENT_3D('',#5492,#3671,#3672);
#2862=AXIS2_PLACEMENT_3D('',#5493,#3673,#3674);
#2863=AXIS2_PLACEMENT_3D('',#5494,#3675,#3676);
#2864=AXIS2_PLACEMENT_3D('',#5495,#3677,#3678);
#2865=AXIS2_PLACEMENT_3D('',#5496,#3679,#3680);
#2866=AXIS2_PLACEMENT_3D('',#5497,#3681,#3682);
#2867=DIRECTION('axis',(0.,0.,1.));
#2868=DIRECTION('refdir',(1.,0.,0.));
#2869=DIRECTION('axis',(0.,0.,1.));
#2870=DIRECTION('refdir',(1.,0.,0.));
#2871=DIRECTION('axis',(0.,0.,1.));
#2872=DIRECTION('refdir',(1.,0.,0.));
#2873=DIRECTION('center_axis',(0.,1.,0.));
#2874=DIRECTION('ref_axis',(1.,0.,0.));
#2875=DIRECTION('center_axis',(0.,1.,0.));
#2876=DIRECTION('ref_axis',(1.,0.,0.));
#2877=DIRECTION('',(0.,1.,0.));
#2878=DIRECTION('center_axis',(0.,-1.,0.));
#2879=DIRECTION('ref_axis',(1.,0.,0.));
#2880=DIRECTION('center_axis',(0.,1.,0.));
#2881=DIRECTION('ref_axis',(1.,0.,0.));
#2882=DIRECTION('center_axis',(0.,1.,0.));
#2883=DIRECTION('ref_axis',(1.,0.,0.));
#2884=DIRECTION('',(0.,1.,0.));
#2885=DIRECTION('center_axis',(0.,-1.,0.));
#2886=DIRECTION('ref_axis',(1.,0.,0.));
#2887=DIRECTION('center_axis',(0.,1.,0.));
#2888=DIRECTION('ref_axis',(1.,0.,0.));
#2889=DIRECTION('center_axis',(0.,1.,0.));
#2890=DIRECTION('ref_axis',(1.,0.,0.));
#2891=DIRECTION('',(0.,1.,0.));
#2892=DIRECTION('center_axis',(0.,-1.,0.));
#2893=DIRECTION('ref_axis',(1.,0.,0.));
#2894=DIRECTION('center_axis',(0.,1.,0.));
#2895=DIRECTION('ref_axis',(1.,0.,0.));
#2896=DIRECTION('center_axis',(0.,1.,0.));
#2897=DIRECTION('ref_axis',(1.,0.,0.));
#2898=DIRECTION('',(0.,1.,0.));
#2899=DIRECTION('center_axis',(0.,-1.,0.));
#2900=DIRECTION('ref_axis',(1.,0.,0.));
#2901=DIRECTION('center_axis',(0.,1.,0.));
#2902=DIRECTION('ref_axis',(1.,0.,0.));
#2903=DIRECTION('center_axis',(0.,1.,0.));
#2904=DIRECTION('ref_axis',(1.,0.,0.));
#2905=DIRECTION('',(0.,1.,0.));
#2906=DIRECTION('center_axis',(0.,-1.,0.));
#2907=DIRECTION('ref_axis',(1.,0.,0.));
#2908=DIRECTION('center_axis',(0.,1.,0.));
#2909=DIRECTION('ref_axis',(1.,0.,0.));
#2910=DIRECTION('center_axis',(0.,1.,0.));
#2911=DIRECTION('ref_axis',(1.,0.,0.));
#2912=DIRECTION('center_axis',(0.,1.,0.));
#2913=DIRECTION('ref_axis',(1.,0.,0.));
#2914=DIRECTION('',(0.,1.,0.));
#2915=DIRECTION('center_axis',(0.,-1.,0.));
#2916=DIRECTION('ref_axis',(1.,0.,0.));
#2917=DIRECTION('center_axis',(0.,1.,0.));
#2918=DIRECTION('ref_axis',(1.,0.,0.));
#2919=DIRECTION('center_axis',(0.,1.,0.));
#2920=DIRECTION('ref_axis',(1.,0.,0.));
#2921=DIRECTION('center_axis',(0.,1.,0.));
#2922=DIRECTION('ref_axis',(1.,0.,0.));
#2923=DIRECTION('',(0.,1.,0.));
#2924=DIRECTION('center_axis',(0.,-1.,0.));
#2925=DIRECTION('ref_axis',(1.,0.,0.));
#2926=DIRECTION('center_axis',(0.,1.,0.));
#2927=DIRECTION('ref_axis',(1.,0.,0.));
#2928=DIRECTION('center_axis',(0.,1.,0.));
#2929=DIRECTION('ref_axis',(1.,0.,0.));
#2930=DIRECTION('center_axis',(0.,1.,0.));
#2931=DIRECTION('ref_axis',(1.,0.,0.));
#2932=DIRECTION('',(0.,1.,0.));
#2933=DIRECTION('center_axis',(0.,-1.,0.));
#2934=DIRECTION('ref_axis',(1.,0.,0.));
#2935=DIRECTION('center_axis',(0.,1.,0.));
#2936=DIRECTION('ref_axis',(1.,0.,0.));
#2937=DIRECTION('center_axis',(0.,1.,0.));
#2938=DIRECTION('ref_axis',(1.,0.,0.));
#2939=DIRECTION('center_axis',(0.,1.,0.));
#2940=DIRECTION('ref_axis',(1.,0.,0.));
#2941=DIRECTION('',(0.,1.,0.));
#2942=DIRECTION('center_axis',(0.,1.,0.));
#2943=DIRECTION('ref_axis',(1.,0.,0.));
#2944=DIRECTION('center_axis',(0.,1.,0.));
#2945=DIRECTION('ref_axis',(1.,0.,0.));
#2946=DIRECTION('center_axis',(0.,1.,0.));
#2947=DIRECTION('ref_axis',(1.,0.,0.));
#2948=DIRECTION('center_axis',(0.,1.,0.));
#2949=DIRECTION('ref_axis',(1.,0.,0.));
#2950=DIRECTION('',(0.,1.,0.));
#2951=DIRECTION('center_axis',(0.,1.,0.));
#2952=DIRECTION('ref_axis',(1.,0.,0.));
#2953=DIRECTION('center_axis',(0.,1.,0.));
#2954=DIRECTION('ref_axis',(1.,0.,0.));
#2955=DIRECTION('center_axis',(0.,1.,0.));
#2956=DIRECTION('ref_axis',(1.,0.,0.));
#2957=DIRECTION('center_axis',(0.,1.,0.));
#2958=DIRECTION('ref_axis',(1.,0.,0.));
#2959=DIRECTION('',(0.,1.,0.));
#2960=DIRECTION('center_axis',(0.,1.,0.));
#2961=DIRECTION('ref_axis',(1.,0.,0.));
#2962=DIRECTION('center_axis',(0.,1.,0.));
#2963=DIRECTION('ref_axis',(1.,0.,0.));
#2964=DIRECTION('center_axis',(0.,1.,0.));
#2965=DIRECTION('ref_axis',(1.,0.,0.));
#2966=DIRECTION('center_axis',(0.,1.,0.));
#2967=DIRECTION('ref_axis',(1.,0.,0.));
#2968=DIRECTION('',(0.,1.,0.));
#2969=DIRECTION('center_axis',(0.,1.,0.));
#2970=DIRECTION('ref_axis',(1.,0.,0.));
#2971=DIRECTION('center_axis',(0.,1.,0.));
#2972=DIRECTION('ref_axis',(1.,0.,0.));
#2973=DIRECTION('center_axis',(0.,1.,0.));
#2974=DIRECTION('ref_axis',(1.,0.,0.));
#2975=DIRECTION('center_axis',(0.,1.,0.));
#2976=DIRECTION('ref_axis',(1.,0.,0.));
#2977=DIRECTION('center_axis',(0.,1.,0.));
#2978=DIRECTION('ref_axis',(1.,0.,0.));
#2979=DIRECTION('center_axis',(0.,1.,0.));
#2980=DIRECTION('ref_axis',(1.,0.,0.));
#2981=DIRECTION('center_axis',(0.,1.,0.));
#2982=DIRECTION('ref_axis',(1.,0.,0.));
#2983=DIRECTION('center_axis',(0.,-1.,0.));
#2984=DIRECTION('ref_axis',(1.,0.,0.));
#2985=DIRECTION('center_axis',(0.,1.,0.));
#2986=DIRECTION('ref_axis',(1.,0.,0.));
#2987=DIRECTION('',(0.,-1.,0.));
#2988=DIRECTION('center_axis',(0.,1.,0.));
#2989=DIRECTION('ref_axis',(1.,0.,0.));
#2990=DIRECTION('',(0.,-1.,0.));
#2991=DIRECTION('center_axis',(0.,1.,0.));
#2992=DIRECTION('ref_axis',(1.,0.,0.));
#2993=DIRECTION('center_axis',(0.,1.,0.));
#2994=DIRECTION('ref_axis',(1.,0.,0.));
#2995=DIRECTION('center_axis',(0.,-1.,0.));
#2996=DIRECTION('ref_axis',(1.,0.,0.));
#2997=DIRECTION('',(0.,-1.,0.));
#2998=DIRECTION('center_axis',(0.,-1.,0.));
#2999=DIRECTION('ref_axis',(1.,0.,0.));
#3000=DIRECTION('center_axis',(0.,1.,0.));
#3001=DIRECTION('ref_axis',(1.,0.,0.));
#3002=DIRECTION('center_axis',(0.,1.,0.));
#3003=DIRECTION('ref_axis',(1.,0.,0.));
#3004=DIRECTION('',(0.,-1.,0.));
#3005=DIRECTION('center_axis',(0.,1.,0.));
#3006=DIRECTION('ref_axis',(1.,0.,0.));
#3007=DIRECTION('center_axis',(0.,1.,0.));
#3008=DIRECTION('ref_axis',(1.,0.,0.));
#3009=DIRECTION('axis',(0.,0.,1.));
#3010=DIRECTION('refdir',(1.,0.,0.));
#3011=DIRECTION('axis',(0.,0.,1.));
#3012=DIRECTION('refdir',(1.,0.,0.));
#3013=DIRECTION('center_axis',(0.,-1.,0.));
#3014=DIRECTION('ref_axis',(0.,0.,-1.));
#3015=DIRECTION('center_axis',(0.,-1.,0.));
#3016=DIRECTION('ref_axis',(1.,0.,0.));
#3017=DIRECTION('center_axis',(0.,-1.,0.));
#3018=DIRECTION('ref_axis',(1.,0.,0.));
#3019=DIRECTION('center_axis',(1.,0.,1.22464679914735E-16));
#3020=DIRECTION('ref_axis',(-1.22464679914735E-16,0.,1.));
#3021=DIRECTION('center_axis',(0.,1.,0.));
#3022=DIRECTION('ref_axis',(1.,0.,0.));
#3023=DIRECTION('center_axis',(0.,1.,0.));
#3024=DIRECTION('ref_axis',(1.,0.,0.));
#3025=DIRECTION('center_axis',(0.,-1.,0.));
#3026=DIRECTION('ref_axis',(1.,0.,0.));
#3027=DIRECTION('',(0.,1.,0.));
#3028=DIRECTION('center_axis',(0.,-1.,0.));
#3029=DIRECTION('ref_axis',(1.,0.,0.));
#3030=DIRECTION('center_axis',(0.,-1.,0.));
#3031=DIRECTION('ref_axis',(1.,0.,0.));
#3032=DIRECTION('center_axis',(0.,-1.,0.));
#3033=DIRECTION('ref_axis',(1.,0.,0.));
#3034=DIRECTION('',(0.,1.,0.));
#3035=DIRECTION('center_axis',(0.,-1.,0.));
#3036=DIRECTION('ref_axis',(1.,0.,0.));
#3037=DIRECTION('center_axis',(0.,1.,0.));
#3038=DIRECTION('ref_axis',(1.,0.,0.));
#3039=DIRECTION('',(-0.707106781186548,0.707106781186547,-8.65956056235494E-17));
#3040=DIRECTION('center_axis',(0.,-1.,0.));
#3041=DIRECTION('ref_axis',(1.,0.,0.));
#3042=DIRECTION('center_axis',(0.,1.,0.));
#3043=DIRECTION('ref_axis',(0.,0.,1.));
#3044=DIRECTION('center_axis',(0.,-1.,0.));
#3045=DIRECTION('ref_axis',(1.,0.,0.));
#3046=DIRECTION('center_axis',(0.,-1.,0.));
#3047=DIRECTION('ref_axis',(1.,0.,0.));
#3048=DIRECTION('',(0.,1.,0.));
#3049=DIRECTION('center_axis',(0.,-1.,0.));
#3050=DIRECTION('ref_axis',(0.,0.,-1.));
#3051=DIRECTION('center_axis',(0.,-1.,0.));
#3052=DIRECTION('ref_axis',(1.,0.,0.));
#3053=DIRECTION('center_axis',(0.,-1.,0.));
#3054=DIRECTION('ref_axis',(1.,0.,0.));
#3055=DIRECTION('',(0.707106781186548,0.707106781186547,8.65956056235494E-17));
#3056=DIRECTION('axis',(0.,0.,1.));
#3057=DIRECTION('refdir',(1.,0.,0.));
#3058=DIRECTION('center_axis',(0.,-1.,0.));
#3059=DIRECTION('ref_axis',(0.,0.,-1.));
#3060=DIRECTION('center_axis',(0.,-1.,0.));
#3061=DIRECTION('ref_axis',(1.,0.,0.));
#3062=DIRECTION('center_axis',(0.,-1.,0.));
#3063=DIRECTION('ref_axis',(1.,0.,0.));
#3064=DIRECTION('center_axis',(1.,0.,1.22464679914735E-16));
#3065=DIRECTION('ref_axis',(-1.22464679914735E-16,0.,1.));
#3066=DIRECTION('center_axis',(0.,1.,0.));
#3067=DIRECTION('ref_axis',(1.,0.,0.));
#3068=DIRECTION('center_axis',(0.,1.,0.));
#3069=DIRECTION('ref_axis',(1.,0.,0.));
#3070=DIRECTION('center_axis',(0.,-1.,0.));
#3071=DIRECTION('ref_axis',(1.,0.,0.));
#3072=DIRECTION('center_axis',(0.,-1.,0.));
#3073=DIRECTION('ref_axis',(1.,0.,0.));
#3074=DIRECTION('',(0.,1.,0.));
#3075=DIRECTION('center_axis',(0.,1.,0.));
#3076=DIRECTION('ref_axis',(0.,0.,1.));
#3077=DIRECTION('center_axis',(0.,-1.,0.));
#3078=DIRECTION('ref_axis',(1.,0.,0.));
#3079=DIRECTION('center_axis',(0.,-1.,0.));
#3080=DIRECTION('ref_axis',(1.,0.,0.));
#3081=DIRECTION('center_axis',(0.,-1.,0.));
#3082=DIRECTION('ref_axis',(1.,0.,0.));
#3083=DIRECTION('center_axis',(0.,-1.,0.));
#3084=DIRECTION('ref_axis',(1.,0.,0.));
#3085=DIRECTION('',(0.707106781186548,0.707106781186547,8.65956056235494E-17));
#3086=DIRECTION('center_axis',(0.,-1.,0.));
#3087=DIRECTION('ref_axis',(1.,0.,0.));
#3088=DIRECTION('center_axis',(0.,-1.,0.));
#3089=DIRECTION('ref_axis',(1.,0.,0.));
#3090=DIRECTION('',(0.,1.,0.));
#3091=DIRECTION('center_axis',(0.,1.,0.));
#3092=DIRECTION('ref_axis',(1.,0.,0.));
#3093=DIRECTION('center_axis',(0.,-1.,0.));
#3094=DIRECTION('ref_axis',(1.,0.,0.));
#3095=DIRECTION('',(-0.707106781186548,0.707106781186547,-8.65956056235494E-17));
#3096=DIRECTION('center_axis',(0.,-1.,0.));
#3097=DIRECTION('ref_axis',(0.,0.,-1.));
#3098=DIRECTION('center_axis',(0.,-1.,0.));
#3099=DIRECTION('ref_axis',(1.,0.,0.));
#3100=DIRECTION('',(0.,1.,0.));
#3101=DIRECTION('axis',(0.,0.,1.));
#3102=DIRECTION('refdir',(1.,0.,0.));
#3103=DIRECTION('center_axis',(0.,0.,1.));
#3104=DIRECTION('ref_axis',(1.,0.,0.));
#3105=DIRECTION('center_axis',(1.22464679914735E-16,-1.,0.));
#3106=DIRECTION('ref_axis',(-1.,-1.22464679914735E-16,0.));
#3107=DIRECTION('center_axis',(0.707106781186548,0.,0.707106781186548));
#3108=DIRECTION('ref_axis',(0.707106781186548,0.,-0.707106781186548));
#3109=DIRECTION('center_axis',(8.65956056235493E-17,-1.,-8.65956056235493E-17));
#3110=DIRECTION('ref_axis',(-0.707106781186548,-1.22464679914735E-16,0.707106781186548));
#3111=DIRECTION('center_axis',(1.,0.,0.));
#3112=DIRECTION('ref_axis',(6.12323399573677E-17,0.,-1.));
#3113=DIRECTION('center_axis',(7.49879891330929E-33,-1.,-1.22464679914735E-16));
#3114=DIRECTION('ref_axis',(-6.12323399573677E-17,-1.22464679914735E-16,
1.));
#3115=DIRECTION('center_axis',(0.707106781186548,0.,-0.707106781186548));
#3116=DIRECTION('ref_axis',(-0.707106781186548,0.,-0.707106781186548));
#3117=DIRECTION('center_axis',(-8.65956056235493E-17,-1.,-8.65956056235493E-17));
#3118=DIRECTION('ref_axis',(0.707106781186548,-1.22464679914735E-16,0.707106781186548));
#3119=DIRECTION('center_axis',(0.,0.,-1.));
#3120=DIRECTION('ref_axis',(-1.,0.,-1.22464679914735E-16));
#3121=DIRECTION('center_axis',(-1.22464679914735E-16,-1.,-1.49975978266186E-32));
#3122=DIRECTION('ref_axis',(1.,-1.22464679914735E-16,1.22464679914735E-16));
#3123=DIRECTION('center_axis',(-0.707106781186548,0.,-0.707106781186548));
#3124=DIRECTION('ref_axis',(-0.707106781186548,0.,0.707106781186548));
#3125=DIRECTION('center_axis',(-8.65956056235493E-17,-1.,8.65956056235493E-17));
#3126=DIRECTION('ref_axis',(0.707106781186548,-1.22464679914735E-16,-0.707106781186548));
#3127=DIRECTION('center_axis',(-1.,0.,0.));
#3128=DIRECTION('ref_axis',(-1.83697019872103E-16,0.,1.));
#3129=DIRECTION('center_axis',(-2.24963967399279E-32,-1.,1.22464679914735E-16));
#3130=DIRECTION('ref_axis',(1.83697019872103E-16,-1.22464679914735E-16,
-1.));
#3131=DIRECTION('center_axis',(-0.707106781186548,0.,0.707106781186548));
#3132=DIRECTION('ref_axis',(0.707106781186548,0.,0.707106781186548));
#3133=DIRECTION('center_axis',(8.65956056235493E-17,-1.,8.65956056235494E-17));
#3134=DIRECTION('ref_axis',(-0.707106781186548,-1.22464679914735E-16,-0.707106781186548));
#3135=DIRECTION('axis',(0.,0.,1.));
#3136=DIRECTION('refdir',(1.,0.,0.));
#3137=DIRECTION('center_axis',(0.,0.,1.));
#3138=DIRECTION('ref_axis',(1.,0.,0.));
#3139=DIRECTION('center_axis',(0.,-1.,0.));
#3140=DIRECTION('ref_axis',(0.,0.,-1.));
#3141=DIRECTION('center_axis',(0.,-1.,0.));
#3142=DIRECTION('ref_axis',(0.,0.,-1.));
#3143=DIRECTION('center_axis',(0.,1.,0.));
#3144=DIRECTION('ref_axis',(1.,0.,0.));
#3145=DIRECTION('center_axis',(0.,1.,0.));
#3146=DIRECTION('ref_axis',(1.,0.,0.));
#3147=DIRECTION('center_axis',(0.,1.,0.));
#3148=DIRECTION('ref_axis',(1.,0.,0.));
#3149=DIRECTION('center_axis',(0.,1.,0.));
#3150=DIRECTION('ref_axis',(1.,0.,0.));
#3151=DIRECTION('',(0.,-1.,0.));
#3152=DIRECTION('center_axis',(0.,-1.,0.));
#3153=DIRECTION('ref_axis',(1.,0.,0.));
#3154=DIRECTION('center_axis',(0.,1.,0.));
#3155=DIRECTION('ref_axis',(1.,0.,0.));
#3156=DIRECTION('center_axis',(0.,1.,0.));
#3157=DIRECTION('ref_axis',(1.,0.,0.));
#3158=DIRECTION('center_axis',(0.,1.,0.));
#3159=DIRECTION('ref_axis',(1.,0.,0.));
#3160=DIRECTION('center_axis',(0.,1.,0.));
#3161=DIRECTION('ref_axis',(1.,0.,0.));
#3162=DIRECTION('center_axis',(0.,1.,0.));
#3163=DIRECTION('ref_axis',(1.,0.,0.));
#3164=DIRECTION('center_axis',(0.,1.,0.));
#3165=DIRECTION('ref_axis',(1.,0.,0.));
#3166=DIRECTION('center_axis',(0.,-1.,0.));
#3167=DIRECTION('ref_axis',(1.,0.,0.));
#3168=DIRECTION('center_axis',(0.,-1.,0.));
#3169=DIRECTION('ref_axis',(0.,0.,-1.));
#3170=DIRECTION('center_axis',(6.12323399573677E-17,0.,1.));
#3171=DIRECTION('ref_axis',(1.,0.,0.));
#3172=DIRECTION('center_axis',(0.,-1.,0.));
#3173=DIRECTION('ref_axis',(0.,0.,-1.));
#3174=DIRECTION('center_axis',(0.,1.,0.));
#3175=DIRECTION('ref_axis',(1.,0.,0.));
#3176=DIRECTION('center_axis',(0.,-1.,0.));
#3177=DIRECTION('ref_axis',(1.,0.,0.));
#3178=DIRECTION('center_axis',(0.,-1.,0.));
#3179=DIRECTION('ref_axis',(0.,0.,-1.));
#3180=DIRECTION('center_axis',(0.,0.,1.));
#3181=DIRECTION('ref_axis',(1.,0.,0.));
#3182=DIRECTION('center_axis',(0.,-1.,0.));
#3183=DIRECTION('ref_axis',(0.,0.,-1.));
#3184=DIRECTION('center_axis',(0.,1.,0.));
#3185=DIRECTION('ref_axis',(1.,0.,0.));
#3186=DIRECTION('center_axis',(0.,-1.,0.));
#3187=DIRECTION('ref_axis',(1.,0.,0.));
#3188=DIRECTION('center_axis',(0.,-1.,0.));
#3189=DIRECTION('ref_axis',(0.,0.,-1.));
#3190=DIRECTION('center_axis',(0.,0.,1.));
#3191=DIRECTION('ref_axis',(1.,0.,0.));
#3192=DIRECTION('center_axis',(0.,-1.,0.));
#3193=DIRECTION('ref_axis',(0.,0.,-1.));
#3194=DIRECTION('center_axis',(0.,1.,0.));
#3195=DIRECTION('ref_axis',(1.,0.,0.));
#3196=DIRECTION('center_axis',(0.,-1.,0.));
#3197=DIRECTION('ref_axis',(1.,0.,0.));
#3198=DIRECTION('center_axis',(0.,-1.,0.));
#3199=DIRECTION('ref_axis',(0.,0.,-1.));
#3200=DIRECTION('center_axis',(0.,0.,1.));
#3201=DIRECTION('ref_axis',(1.,0.,0.));
#3202=DIRECTION('center_axis',(0.,-1.,0.));
#3203=DIRECTION('ref_axis',(0.,0.,-1.));
#3204=DIRECTION('center_axis',(0.,1.,0.));
#3205=DIRECTION('ref_axis',(1.,0.,0.));
#3206=DIRECTION('center_axis',(0.,-1.,0.));
#3207=DIRECTION('ref_axis',(1.,0.,0.));
#3208=DIRECTION('center_axis',(0.,-1.,0.));
#3209=DIRECTION('ref_axis',(0.,0.,-1.));
#3210=DIRECTION('center_axis',(6.12323399573676E-17,0.,1.));
#3211=DIRECTION('ref_axis',(1.,0.,0.));
#3212=DIRECTION('center_axis',(0.,-1.,0.));
#3213=DIRECTION('ref_axis',(0.,0.,-1.));
#3214=DIRECTION('center_axis',(0.,1.,0.));
#3215=DIRECTION('ref_axis',(1.,0.,0.));
#3216=DIRECTION('center_axis',(0.,-1.,0.));
#3217=DIRECTION('ref_axis',(1.,0.,0.));
#3218=DIRECTION('center_axis',(0.,-1.,0.));
#3219=DIRECTION('ref_axis',(0.,0.,-1.));
#3220=DIRECTION('center_axis',(0.,0.,1.));
#3221=DIRECTION('ref_axis',(1.,0.,0.));
#3222=DIRECTION('center_axis',(0.,-1.,0.));
#3223=DIRECTION('ref_axis',(0.,0.,-1.));
#3224=DIRECTION('center_axis',(0.,1.,0.));
#3225=DIRECTION('ref_axis',(1.,0.,0.));
#3226=DIRECTION('center_axis',(0.,1.,0.));
#3227=DIRECTION('ref_axis',(1.,0.,0.));
#3228=DIRECTION('',(0.,1.,0.));
#3229=DIRECTION('center_axis',(0.,-1.,0.));
#3230=DIRECTION('ref_axis',(1.,0.,0.));
#3231=DIRECTION('center_axis',(0.,-1.,0.));
#3232=DIRECTION('ref_axis',(1.,0.,0.));
#3233=DIRECTION('center_axis',(0.,1.,0.));
#3234=DIRECTION('ref_axis',(1.,0.,0.));
#3235=DIRECTION('center_axis',(0.,-1.,0.));
#3236=DIRECTION('ref_axis',(0.,0.,-1.));
#3237=DIRECTION('center_axis',(0.,0.,1.));
#3238=DIRECTION('ref_axis',(1.,0.,0.));
#3239=DIRECTION('center_axis',(0.,-1.,0.));
#3240=DIRECTION('ref_axis',(0.,0.,-1.));
#3241=DIRECTION('center_axis',(0.,-1.,0.));
#3242=DIRECTION('ref_axis',(-1.,0.,0.));
#3243=DIRECTION('center_axis',(0.,1.,0.));
#3244=DIRECTION('ref_axis',(1.,0.,0.));
#3245=DIRECTION('axis',(0.,0.,1.));
#3246=DIRECTION('refdir',(1.,0.,0.));
#3247=DIRECTION('center_axis',(0.,1.,0.));
#3248=DIRECTION('ref_axis',(0.,0.,1.));
#3249=DIRECTION('center_axis',(0.,-1.,0.));
#3250=DIRECTION('ref_axis',(1.,0.,0.));
#3251=DIRECTION('center_axis',(0.,-1.,0.));
#3252=DIRECTION('ref_axis',(1.,0.,0.));
#3253=DIRECTION('center_axis',(0.,-1.,0.));
#3254=DIRECTION('ref_axis',(1.,0.,0.));
#3255=DIRECTION('center_axis',(0.,-1.,0.));
#3256=DIRECTION('ref_axis',(1.,0.,0.));
#3257=DIRECTION('',(0.,1.,0.));
#3258=DIRECTION('center_axis',(0.,-1.,0.));
#3259=DIRECTION('ref_axis',(0.,0.,-1.));
#3260=DIRECTION('center_axis',(0.,-1.,0.));
#3261=DIRECTION('ref_axis',(1.,0.,0.));
#3262=DIRECTION('center_axis',(0.,-1.,0.));
#3263=DIRECTION('ref_axis',(1.,0.,0.));
#3264=DIRECTION('',(0.,1.,0.));
#3265=DIRECTION('center_axis',(0.,1.,0.));
#3266=DIRECTION('ref_axis',(0.,0.,1.));
#3267=DIRECTION('center_axis',(0.,-1.,0.));
#3268=DIRECTION('ref_axis',(1.,0.,0.));
#3269=DIRECTION('center_axis',(0.,-1.,0.));
#3270=DIRECTION('ref_axis',(1.,0.,0.));
#3271=DIRECTION('center_axis',(0.,-1.,0.));
#3272=DIRECTION('ref_axis',(1.,0.,0.));
#3273=DIRECTION('center_axis',(0.,-1.,0.));
#3274=DIRECTION('ref_axis',(1.,0.,0.));
#3275=DIRECTION('',(0.,1.,0.));
#3276=DIRECTION('center_axis',(0.,-1.,0.));
#3277=DIRECTION('ref_axis',(0.,0.,-1.));
#3278=DIRECTION('center_axis',(0.,-1.,0.));
#3279=DIRECTION('ref_axis',(1.,0.,0.));
#3280=DIRECTION('center_axis',(0.,-1.,0.));
#3281=DIRECTION('ref_axis',(1.,0.,0.));
#3282=DIRECTION('',(0.,1.,0.));
#3283=DIRECTION('',(0.,0.,1.));
#3284=DIRECTION('',(1.,0.,0.));
#3285=DIRECTION('',(0.,0.,1.));
#3286=DIRECTION('',(1.,0.,0.));
#3287=DIRECTION('',(0.,0.,1.));
#3288=DIRECTION('',(1.,0.,0.));
#3289=DIRECTION('',(0.,0.,1.));
#3290=DIRECTION('',(1.,0.,0.));
#3291=DIRECTION('',(0.,0.,1.));
#3292=DIRECTION('',(1.,0.,0.));
#3293=DIRECTION('axis',(0.,0.,1.));
#3294=DIRECTION('refdir',(1.,0.,0.));
#3295=DIRECTION('center_axis',(0.,1.,0.));
#3296=DIRECTION('ref_axis',(1.,0.,0.));
#3297=DIRECTION('center_axis',(0.,-1.,0.));
#3298=DIRECTION('ref_axis',(1.,0.,0.));
#3299=DIRECTION('',(0.,-1.,0.));
#3300=DIRECTION('center_axis',(0.,-1.,0.));
#3301=DIRECTION('ref_axis',(1.,0.,0.));
#3302=DIRECTION('center_axis',(0.,1.,0.));
#3303=DIRECTION('ref_axis',(1.,0.,0.));
#3304=DIRECTION('center_axis',(0.,1.,0.));
#3305=DIRECTION('ref_axis',(1.,0.,0.));
#3306=DIRECTION('',(0.,-1.,0.));
#3307=DIRECTION('center_axis',(0.,1.,0.));
#3308=DIRECTION('ref_axis',(1.,0.,0.));
#3309=DIRECTION('center_axis',(0.,1.,0.));
#3310=DIRECTION('ref_axis',(1.,0.,0.));
#3311=DIRECTION('center_axis',(0.,1.,0.));
#3312=DIRECTION('ref_axis',(1.,0.,0.));
#3313=DIRECTION('axis',(0.,0.,1.));
#3314=DIRECTION('refdir',(1.,0.,0.));
#3315=DIRECTION('center_axis',(0.,1.,0.));
#3316=DIRECTION('ref_axis',(1.,0.,0.));
#3317=DIRECTION('center_axis',(0.,1.,0.));
#3318=DIRECTION('ref_axis',(1.,0.,0.));
#3319=DIRECTION('',(0.,1.,0.));
#3320=DIRECTION('center_axis',(0.,-1.,0.));
#3321=DIRECTION('ref_axis',(1.,0.,0.));
#3322=DIRECTION('center_axis',(0.,1.,0.));
#3323=DIRECTION('ref_axis',(1.,0.,0.));
#3324=DIRECTION('center_axis',(0.,1.,0.));
#3325=DIRECTION('ref_axis',(1.,0.,0.));
#3326=DIRECTION('',(0.,1.,0.));
#3327=DIRECTION('center_axis',(0.,-1.,0.));
#3328=DIRECTION('ref_axis',(1.,0.,0.));
#3329=DIRECTION('center_axis',(0.,1.,0.));
#3330=DIRECTION('ref_axis',(1.,0.,0.));
#3331=DIRECTION('center_axis',(0.,1.,0.));
#3332=DIRECTION('ref_axis',(1.,0.,0.));
#3333=DIRECTION('',(0.,1.,0.));
#3334=DIRECTION('center_axis',(0.,-1.,0.));
#3335=DIRECTION('ref_axis',(1.,0.,0.));
#3336=DIRECTION('center_axis',(0.,1.,0.));
#3337=DIRECTION('ref_axis',(1.,0.,0.));
#3338=DIRECTION('center_axis',(0.,1.,0.));
#3339=DIRECTION('ref_axis',(1.,0.,0.));
#3340=DIRECTION('',(0.,1.,0.));
#3341=DIRECTION('center_axis',(0.,-1.,0.));
#3342=DIRECTION('ref_axis',(1.,0.,0.));
#3343=DIRECTION('center_axis',(0.,1.,0.));
#3344=DIRECTION('ref_axis',(1.,0.,0.));
#3345=DIRECTION('center_axis',(0.,1.,0.));
#3346=DIRECTION('ref_axis',(1.,0.,0.));
#3347=DIRECTION('',(0.,-1.,0.));
#3348=DIRECTION('center_axis',(0.,-1.,0.));
#3349=DIRECTION('ref_axis',(1.,0.,0.));
#3350=DIRECTION('center_axis',(0.,1.,0.));
#3351=DIRECTION('ref_axis',(1.,0.,0.));
#3352=DIRECTION('center_axis',(0.,-1.,0.));
#3353=DIRECTION('ref_axis',(1.,0.,0.));
#3354=DIRECTION('center_axis',(0.,1.,0.));
#3355=DIRECTION('ref_axis',(1.,0.,0.));
#3356=DIRECTION('center_axis',(0.,1.,0.));
#3357=DIRECTION('ref_axis',(1.,0.,0.));
#3358=DIRECTION('',(0.,1.,0.));
#3359=DIRECTION('center_axis',(0.,1.,0.));
#3360=DIRECTION('ref_axis',(1.,0.,0.));
#3361=DIRECTION('center_axis',(0.,1.,0.));
#3362=DIRECTION('ref_axis',(1.,0.,0.));
#3363=DIRECTION('center_axis',(0.,-1.,0.));
#3364=DIRECTION('ref_axis',(1.,0.,0.));
#3365=DIRECTION('center_axis',(0.,1.,0.));
#3366=DIRECTION('ref_axis',(1.,0.,0.));
#3367=DIRECTION('',(0.,-1.,0.));
#3368=DIRECTION('center_axis',(0.,1.,0.));
#3369=DIRECTION('ref_axis',(1.,0.,0.));
#3370=DIRECTION('center_axis',(0.,1.,0.));
#3371=DIRECTION('ref_axis',(1.,0.,0.));
#3372=DIRECTION('',(0.,-1.,0.));
#3373=DIRECTION('center_axis',(0.,1.,0.));
#3374=DIRECTION('ref_axis',(1.,0.,0.));
#3375=DIRECTION('center_axis',(0.,1.,0.));
#3376=DIRECTION('ref_axis',(1.,0.,0.));
#3377=DIRECTION('center_axis',(0.,1.,0.));
#3378=DIRECTION('ref_axis',(1.,0.,0.));
#3379=DIRECTION('axis',(0.,0.,1.));
#3380=DIRECTION('refdir',(1.,0.,0.));
#3381=DIRECTION('center_axis',(0.,1.,0.));
#3382=DIRECTION('ref_axis',(1.,0.,0.));
#3383=DIRECTION('center_axis',(0.,-1.,0.));
#3384=DIRECTION('ref_axis',(1.,0.,0.));
#3385=DIRECTION('',(0.,-1.,0.));
#3386=DIRECTION('center_axis',(0.,-1.,0.));
#3387=DIRECTION('ref_axis',(1.,0.,0.));
#3388=DIRECTION('center_axis',(0.,1.,0.));
#3389=DIRECTION('ref_axis',(1.,0.,0.));
#3390=DIRECTION('center_axis',(0.,1.,0.));
#3391=DIRECTION('ref_axis',(1.,0.,0.));
#3392=DIRECTION('',(0.,-1.,0.));
#3393=DIRECTION('center_axis',(0.,1.,0.));
#3394=DIRECTION('ref_axis',(1.,0.,0.));
#3395=DIRECTION('center_axis',(0.,1.,0.));
#3396=DIRECTION('ref_axis',(1.,0.,0.));
#3397=DIRECTION('center_axis',(0.,1.,0.));
#3398=DIRECTION('ref_axis',(1.,0.,0.));
#3399=DIRECTION('axis',(0.,0.,1.));
#3400=DIRECTION('refdir',(1.,0.,0.));
#3401=DIRECTION('center_axis',(0.,1.,0.));
#3402=DIRECTION('ref_axis',(1.,0.,0.));
#3403=DIRECTION('center_axis',(0.,1.,0.));
#3404=DIRECTION('ref_axis',(1.,0.,0.));
#3405=DIRECTION('',(0.,1.,0.));
#3406=DIRECTION('center_axis',(0.,-1.,0.));
#3407=DIRECTION('ref_axis',(1.,0.,0.));
#3408=DIRECTION('center_axis',(0.,1.,0.));
#3409=DIRECTION('ref_axis',(1.,0.,0.));
#3410=DIRECTION('center_axis',(0.,1.,0.));
#3411=DIRECTION('ref_axis',(1.,0.,0.));
#3412=DIRECTION('',(0.,1.,0.));
#3413=DIRECTION('center_axis',(0.,-1.,0.));
#3414=DIRECTION('ref_axis',(1.,0.,0.));
#3415=DIRECTION('center_axis',(0.,1.,0.));
#3416=DIRECTION('ref_axis',(1.,0.,0.));
#3417=DIRECTION('center_axis',(0.,1.,0.));
#3418=DIRECTION('ref_axis',(1.,0.,0.));
#3419=DIRECTION('',(0.,1.,0.));
#3420=DIRECTION('center_axis',(0.,-1.,0.));
#3421=DIRECTION('ref_axis',(1.,0.,0.));
#3422=DIRECTION('center_axis',(0.,1.,0.));
#3423=DIRECTION('ref_axis',(1.,0.,0.));
#3424=DIRECTION('center_axis',(0.,1.,0.));
#3425=DIRECTION('ref_axis',(1.,0.,0.));
#3426=DIRECTION('',(0.,1.,0.));
#3427=DIRECTION('center_axis',(0.,-1.,0.));
#3428=DIRECTION('ref_axis',(1.,0.,0.));
#3429=DIRECTION('center_axis',(0.,1.,0.));
#3430=DIRECTION('ref_axis',(1.,0.,0.));
#3431=DIRECTION('center_axis',(0.,1.,0.));
#3432=DIRECTION('ref_axis',(1.,0.,0.));
#3433=DIRECTION('',(0.,-1.,0.));
#3434=DIRECTION('center_axis',(0.,1.,0.));
#3435=DIRECTION('ref_axis',(1.,0.,0.));
#3436=DIRECTION('center_axis',(0.,1.,0.));
#3437=DIRECTION('ref_axis',(1.,0.,0.));
#3438=DIRECTION('center_axis',(0.,-1.,0.));
#3439=DIRECTION('ref_axis',(1.,0.,0.));
#3440=DIRECTION('center_axis',(0.,1.,0.));
#3441=DIRECTION('ref_axis',(1.,0.,0.));
#3442=DIRECTION('center_axis',(0.,-1.,0.));
#3443=DIRECTION('ref_axis',(1.,0.,0.));
#3444=DIRECTION('',(0.,-1.,0.));
#3445=DIRECTION('center_axis',(0.,1.,0.));
#3446=DIRECTION('ref_axis',(1.,0.,0.));
#3447=DIRECTION('center_axis',(0.,1.,0.));
#3448=DIRECTION('ref_axis',(1.,0.,0.));
#3449=DIRECTION('',(0.,-1.,0.));
#3450=DIRECTION('center_axis',(0.,1.,0.));
#3451=DIRECTION('ref_axis',(1.,0.,0.));
#3452=DIRECTION('center_axis',(0.,1.,0.));
#3453=DIRECTION('ref_axis',(1.,0.,0.));
#3454=DIRECTION('center_axis',(0.,1.,0.));
#3455=DIRECTION('ref_axis',(1.,0.,0.));
#3456=DIRECTION('axis',(0.,0.,1.));
#3457=DIRECTION('refdir',(1.,0.,0.));
#3458=DIRECTION('center_axis',(0.,1.,0.));
#3459=DIRECTION('ref_axis',(0.,0.,1.));
#3460=DIRECTION('center_axis',(0.,-1.,0.));
#3461=DIRECTION('ref_axis',(1.,0.,0.));
#3462=DIRECTION('center_axis',(0.,-1.,0.));
#3463=DIRECTION('ref_axis',(1.,0.,0.));
#3464=DIRECTION('center_axis',(0.,-1.,0.));
#3465=DIRECTION('ref_axis',(1.,0.,0.));
#3466=DIRECTION('',(0.707106781186547,0.707106781186548,8.65956056235493E-17));
#3467=DIRECTION('center_axis',(0.,-1.,0.));
#3468=DIRECTION('ref_axis',(1.,0.,0.));
#3469=DIRECTION('center_axis',(0.,-1.,0.));
#3470=DIRECTION('ref_axis',(1.,0.,0.));
#3471=DIRECTION('',(0.,1.,0.));
#3472=DIRECTION('center_axis',(0.,1.,0.));
#3473=DIRECTION('ref_axis',(1.,0.,0.));
#3474=DIRECTION('center_axis',(0.,-1.,0.));
#3475=DIRECTION('ref_axis',(1.,0.,0.));
#3476=DIRECTION('',(-0.707106781186547,0.707106781186548,-8.65956056235493E-17));
#3477=DIRECTION('center_axis',(0.,-1.,0.));
#3478=DIRECTION('ref_axis',(0.,0.,-1.));
#3479=DIRECTION('center_axis',(0.,-1.,0.));
#3480=DIRECTION('ref_axis',(1.,0.,0.));
#3481=DIRECTION('center_axis',(0.,1.,0.));
#3482=DIRECTION('ref_axis',(1.,0.,0.));
#3483=DIRECTION('center_axis',(0.,1.,0.));
#3484=DIRECTION('ref_axis',(1.,0.,0.));
#3485=DIRECTION('',(-0.447213595499958,0.894427190999916,-5.47678698264203E-17));
#3486=DIRECTION('center_axis',(0.,-1.,0.));
#3487=DIRECTION('ref_axis',(1.,0.,0.));
#3488=DIRECTION('center_axis',(0.,1.,0.));
#3489=DIRECTION('ref_axis',(1.,0.,0.));
#3490=DIRECTION('',(0.,1.,0.));
#3491=DIRECTION('center_axis',(0.,1.,0.));
#3492=DIRECTION('ref_axis',(1.,0.,0.));
#3493=DIRECTION('center_axis',(0.,-1.,0.));
#3494=DIRECTION('ref_axis',(1.,0.,0.));
#3495=DIRECTION('',(-0.707106781186547,0.707106781186548,-8.65956056235493E-17));
#3496=DIRECTION('center_axis',(0.,-1.,0.));
#3497=DIRECTION('ref_axis',(0.,0.,-1.));
#3498=DIRECTION('center_axis',(0.866025403784439,0.,-0.5));
#3499=DIRECTION('ref_axis',(0.5,0.,0.866025403784439));
#3500=DIRECTION('',(-0.5,0.,-0.866025403784439));
#3501=DIRECTION('',(0.,-1.,0.));
#3502=DIRECTION('',(0.5,0.,0.866025403784439));
#3503=DIRECTION('',(0.,-1.,0.));
#3504=DIRECTION('center_axis',(1.60246890531964E-16,0.,-1.));
#3505=DIRECTION('ref_axis',(1.,0.,1.60246890531964E-16));
#3506=DIRECTION('',(-1.,0.,-1.60246890531964E-16));
#3507=DIRECTION('',(0.,-1.,0.));
#3508=DIRECTION('',(1.,0.,1.60246890531964E-16));
#3509=DIRECTION('center_axis',(-0.866025403784439,0.,-0.5));
#3510=DIRECTION('ref_axis',(0.5,0.,-0.866025403784439));
#3511=DIRECTION('',(-0.5,0.,0.866025403784439));
#3512=DIRECTION('',(0.,-1.,0.));
#3513=DIRECTION('',(0.5,0.,-0.866025403784439));
#3514=DIRECTION('center_axis',(-0.866025403784439,0.,0.5));
#3515=DIRECTION('ref_axis',(-0.5,0.,-0.866025403784439));
#3516=DIRECTION('',(0.5,0.,0.866025403784439));
#3517=DIRECTION('',(0.,-1.,0.));
#3518=DIRECTION('',(-0.5,0.,-0.866025403784439));
#3519=DIRECTION('center_axis',(-1.60246890531964E-16,0.,1.));
#3520=DIRECTION('ref_axis',(-1.,0.,-1.60246890531964E-16));
#3521=DIRECTION('',(1.,0.,1.60246890531964E-16));
#3522=DIRECTION('',(0.,-1.,0.));
#3523=DIRECTION('',(-1.,0.,-1.60246890531964E-16));
#3524=DIRECTION('center_axis',(0.866025403784439,0.,0.5));
#3525=DIRECTION('ref_axis',(-0.5,0.,0.866025403784439));
#3526=DIRECTION('',(0.5,0.,-0.866025403784439));
#3527=DIRECTION('',(-0.5,0.,0.866025403784439));
#3528=DIRECTION('center_axis',(0.,1.,0.));
#3529=DIRECTION('ref_axis',(1.,0.,0.));
#3530=DIRECTION('center_axis',(0.,-1.,0.));
#3531=DIRECTION('ref_axis',(0.,0.,-1.));
#3532=DIRECTION('',(0.,0.,1.));
#3533=DIRECTION('',(1.,0.,0.));
#3534=DIRECTION('',(0.,0.,1.));
#3535=DIRECTION('',(1.,0.,0.));
#3536=DIRECTION('',(0.,0.,1.));
#3537=DIRECTION('',(1.,0.,0.));
#3538=DIRECTION('',(0.,0.,1.));
#3539=DIRECTION('',(1.,0.,0.));
#3540=DIRECTION('',(0.,0.,1.));
#3541=DIRECTION('',(1.,0.,0.));
#3542=DIRECTION('',(0.,0.,1.));
#3543=DIRECTION('',(1.,0.,0.));
#3544=DIRECTION('',(0.,0.,1.));
#3545=DIRECTION('',(1.,0.,0.));
#3546=DIRECTION('',(0.,0.,1.));
#3547=DIRECTION('',(-1.,1.22464679914735E-16,0.));
#3548=DIRECTION('',(0.,0.,1.));
#3549=DIRECTION('',(1.,0.,0.));
#3550=DIRECTION('',(0.,0.,1.));
#3551=DIRECTION('',(-1.,1.22464679914735E-16,0.));
#3552=DIRECTION('',(0.,0.,1.));
#3553=DIRECTION('',(1.,0.,0.));
#3554=DIRECTION('',(0.,0.,1.));
#3555=DIRECTION('',(-1.,1.22464679914735E-16,0.));
#3556=DIRECTION('',(0.,0.,1.));
#3557=DIRECTION('',(1.,0.,0.));
#3558=DIRECTION('',(0.,0.,1.));
#3559=DIRECTION('',(-1.,1.22464679914735E-16,0.));
#3560=DIRECTION('',(0.,0.,1.));
#3561=DIRECTION('',(1.,0.,0.));
#3562=DIRECTION('axis',(0.,0.,1.));
#3563=DIRECTION('refdir',(1.,0.,0.));
#3564=DIRECTION('axis',(0.,0.,1.));
#3565=DIRECTION('refdir',(1.,0.,0.));
#3566=DIRECTION('center_axis',(0.,1.,0.));
#3567=DIRECTION('ref_axis',(1.,0.,0.));
#3568=DIRECTION('center_axis',(0.,-1.,0.));
#3569=DIRECTION('ref_axis',(1.,0.,0.));
#3570=DIRECTION('',(0.,1.,0.));
#3571=DIRECTION('center_axis',(0.,-1.,0.));
#3572=DIRECTION('ref_axis',(1.,0.,0.));
#3573=DIRECTION('center_axis',(0.,1.,0.));
#3574=DIRECTION('ref_axis',(1.,0.,0.));
#3575=DIRECTION('center_axis',(0.,1.,0.));
#3576=DIRECTION('ref_axis',(1.,0.,0.));
#3577=DIRECTION('center_axis',(0.,1.,0.));
#3578=DIRECTION('ref_axis',(1.,0.,0.));
#3579=DIRECTION('center_axis',(0.,-1.,0.));
#3580=DIRECTION('ref_axis',(1.,0.,0.));
#3581=DIRECTION('center_axis',(0.,1.,0.));
#3582=DIRECTION('ref_axis',(1.,0.,0.));
#3583=DIRECTION('',(0.,-1.,0.));
#3584=DIRECTION('center_axis',(0.,1.,0.));
#3585=DIRECTION('ref_axis',(1.,0.,0.));
#3586=DIRECTION('center_axis',(0.,1.,0.));
#3587=DIRECTION('ref_axis',(1.,0.,0.));
#3588=DIRECTION('center_axis',(0.,1.,0.));
#3589=DIRECTION('ref_axis',(1.,0.,0.));
#3590=DIRECTION('center_axis',(0.,1.,0.));
#3591=DIRECTION('ref_axis',(1.,0.,0.));
#3592=DIRECTION('center_axis',(0.,1.,0.));
#3593=DIRECTION('ref_axis',(1.,0.,0.));
#3594=DIRECTION('center_axis',(0.,-1.,0.));
#3595=DIRECTION('ref_axis',(1.,0.,0.));
#3596=DIRECTION('center_axis',(0.,1.,0.));
#3597=DIRECTION('ref_axis',(1.,0.,0.));
#3598=DIRECTION('',(0.,-1.,0.));
#3599=DIRECTION('center_axis',(0.,1.,0.));
#3600=DIRECTION('ref_axis',(1.,0.,0.));
#3601=DIRECTION('',(0.,-1.,0.));
#3602=DIRECTION('center_axis',(0.,1.,0.));
#3603=DIRECTION('ref_axis',(1.,0.,0.));
#3604=DIRECTION('center_axis',(0.,1.,0.));
#3605=DIRECTION('ref_axis',(1.,0.,0.));
#3606=DIRECTION('center_axis',(0.,1.,0.));
#3607=DIRECTION('ref_axis',(1.,0.,0.));
#3608=DIRECTION('',(0.,-1.,0.));
#3609=DIRECTION('center_axis',(0.,1.,0.));
#3610=DIRECTION('ref_axis',(1.,0.,0.));
#3611=DIRECTION('center_axis',(0.,1.,0.));
#3612=DIRECTION('ref_axis',(1.,0.,0.));
#3613=DIRECTION('axis',(0.,0.,1.));
#3614=DIRECTION('refdir',(1.,0.,0.));
#3615=DIRECTION('center_axis',(0.,1.,0.));
#3616=DIRECTION('ref_axis',(1.,0.,0.));
#3617=DIRECTION('center_axis',(0.,-1.,0.));
#3618=DIRECTION('ref_axis',(1.,0.,0.));
#3619=DIRECTION('',(0.,-1.,0.));
#3620=DIRECTION('center_axis',(0.,-1.,0.));
#3621=DIRECTION('ref_axis',(1.,0.,0.));
#3622=DIRECTION('center_axis',(0.,1.,0.));
#3623=DIRECTION('ref_axis',(1.,0.,0.));
#3624=DIRECTION('center_axis',(0.,1.,0.));
#3625=DIRECTION('ref_axis',(1.,0.,0.));
#3626=DIRECTION('',(0.,-1.,0.));
#3627=DIRECTION('center_axis',(0.,1.,0.));
#3628=DIRECTION('ref_axis',(1.,0.,0.));
#3629=DIRECTION('center_axis',(0.,1.,0.));
#3630=DIRECTION('ref_axis',(1.,0.,0.));
#3631=DIRECTION('center_axis',(0.,1.,0.));
#3632=DIRECTION('ref_axis',(1.,0.,0.));
#3633=DIRECTION('axis',(0.,0.,1.));
#3634=DIRECTION('refdir',(1.,0.,0.));
#3635=DIRECTION('center_axis',(0.,0.,1.));
#3636=DIRECTION('ref_axis',(1.,0.,0.));
#3637=DIRECTION('',(0.,0.,1.));
#3638=DIRECTION('center_axis',(0.,0.,1.));
#3639=DIRECTION('ref_axis',(1.,0.,0.));
#3640=DIRECTION('',(0.,0.,-1.));
#3641=DIRECTION('center_axis',(0.,0.,-1.));
#3642=DIRECTION('ref_axis',(1.,0.,0.));
#3643=DIRECTION('center_axis',(0.,0.,1.));
#3644=DIRECTION('ref_axis',(-0.998199433392819,-0.0599824238777901,0.));
#3645=DIRECTION('center_axis',(0.,0.,1.));
#3646=DIRECTION('ref_axis',(1.,0.,0.));
#3647=DIRECTION('center_axis',(0.,0.,1.));
#3648=DIRECTION('ref_axis',(1.,0.,0.));
#3649=DIRECTION('center_axis',(0.,0.,1.));
#3650=DIRECTION('ref_axis',(1.,0.,0.));
#3651=DIRECTION('center_axis',(0.,0.,1.));
#3652=DIRECTION('ref_axis',(1.,0.,0.));
#3653=DIRECTION('center_axis',(0.,0.,1.));
#3654=DIRECTION('ref_axis',(1.,0.,0.));
#3655=DIRECTION('center_axis',(0.,0.,1.));
#3656=DIRECTION('ref_axis',(1.,0.,0.));
#3657=DIRECTION('center_axis',(0.,0.,1.));
#3658=DIRECTION('ref_axis',(1.,0.,0.));
#3659=DIRECTION('',(0.,0.,1.));
#3660=DIRECTION('center_axis',(0.,0.,-1.));
#3661=DIRECTION('ref_axis',(1.,0.,0.));
#3662=DIRECTION('center_axis',(0.,0.,1.));
#3663=DIRECTION('ref_axis',(1.,0.,0.));
#3664=DIRECTION('',(0.,0.,1.));
#3665=DIRECTION('center_axis',(0.,0.,-1.));
#3666=DIRECTION('ref_axis',(1.,0.,0.));
#3667=DIRECTION('center_axis',(0.,0.,1.));
#3668=DIRECTION('ref_axis',(-0.998199433392758,0.0599824238788159,0.));
#3669=DIRECTION('center_axis',(0.,0.,1.));
#3670=DIRECTION('ref_axis',(1.,0.,0.));
#3671=DIRECTION('center_axis',(0.,0.,1.));
#3672=DIRECTION('ref_axis',(1.,0.,0.));
#3673=DIRECTION('',(0.,0.,1.));
#3674=DIRECTION('',(1.,0.,0.));
#3675=DIRECTION('',(0.,0.,1.));
#3676=DIRECTION('',(1.,0.,0.));
#3677=DIRECTION('',(0.,-1.,2.22044604925031E-16));
#3678=DIRECTION('',(1.,0.,0.));
#3679=DIRECTION('',(0.,0.,1.));
#3680=DIRECTION('',(1.,0.,0.));
#3681=DIRECTION('',(0.,0.,1.));
#3682=DIRECTION('',(1.,0.,0.));
#3683=CARTESIAN_POINT('',(0.,0.,0.));
#3684=CARTESIAN_POINT('',(0.,0.,0.));
#3685=CARTESIAN_POINT('',(0.,0.,0.));
#3686=CARTESIAN_POINT('Origin',(-2.9698484809835,1.9,1.5301515190165));
#3687=CARTESIAN_POINT('',(-3.4098484809835,2.,1.5301515190165));
#3688=CARTESIAN_POINT('Origin',(-2.9698484809835,2.,1.5301515190165));
#3689=CARTESIAN_POINT('',(-3.4098484809835,2.8,1.5301515190165));
#3690=CARTESIAN_POINT('',(-3.4098484809835,1.9,1.5301515190165));
#3691=CARTESIAN_POINT('Origin',(-2.9698484809835,2.8,1.5301515190165));
#3692=CARTESIAN_POINT('Origin',(-2.9698484809835,1.9,7.4698484809835));
#3693=CARTESIAN_POINT('',(-3.4098484809835,2.,7.4698484809835));
#3694=CARTESIAN_POINT('Origin',(-2.9698484809835,2.,7.4698484809835));
#3695=CARTESIAN_POINT('',(-3.4098484809835,2.8,7.4698484809835));
#3696=CARTESIAN_POINT('',(-3.4098484809835,1.9,7.4698484809835));
#3697=CARTESIAN_POINT('Origin',(-2.9698484809835,2.8,7.4698484809835));
#3698=CARTESIAN_POINT('Origin',(2.9698484809835,1.9,7.4698484809835));
#3699=CARTESIAN_POINT('',(2.5298484809835,2.,7.4698484809835));
#3700=CARTESIAN_POINT('Origin',(2.9698484809835,2.,7.4698484809835));
#3701=CARTESIAN_POINT('',(2.5298484809835,2.8,7.4698484809835));
#3702=CARTESIAN_POINT('',(2.5298484809835,1.9,7.4698484809835));
#3703=CARTESIAN_POINT('Origin',(2.9698484809835,2.8,7.4698484809835));
#3704=CARTESIAN_POINT('Origin',(2.9698484809835,1.9,1.5301515190165));
#3705=CARTESIAN_POINT('',(2.5298484809835,2.,1.5301515190165));
#3706=CARTESIAN_POINT('Origin',(2.9698484809835,2.,1.5301515190165));
#3707=CARTESIAN_POINT('',(2.5298484809835,2.8,1.5301515190165));
#3708=CARTESIAN_POINT('',(2.5298484809835,1.9,1.5301515190165));
#3709=CARTESIAN_POINT('Origin',(2.9698484809835,2.8,1.5301515190165));
#3710=CARTESIAN_POINT('Origin',(-2.8,4.4,4.5));
#3711=CARTESIAN_POINT('',(-2.965,4.4,4.5));
#3712=CARTESIAN_POINT('Origin',(-2.8,4.4,4.5));
#3713=CARTESIAN_POINT('',(-2.965,6.,4.5));
#3714=CARTESIAN_POINT('',(-2.965,4.4,4.5));
#3715=CARTESIAN_POINT('Origin',(-2.8,6.,4.5));
#3716=CARTESIAN_POINT('Origin',(-2.8,4.4,4.5));
#3717=CARTESIAN_POINT('Origin',(1.71450551880629E-16,4.4,7.3));
#3718=CARTESIAN_POINT('',(-0.165,4.4,7.3));
#3719=CARTESIAN_POINT('Origin',(1.71450551880629E-16,4.4,7.3));
#3720=CARTESIAN_POINT('',(-0.165,6.,7.3));
#3721=CARTESIAN_POINT('',(-0.165,4.4,7.3));
#3722=CARTESIAN_POINT('Origin',(1.71450551880629E-16,6.,7.3));
#3723=CARTESIAN_POINT('Origin',(1.66533453693773E-16,4.4,7.3));
#3724=CARTESIAN_POINT('Origin',(2.8,4.4,4.5));
#3725=CARTESIAN_POINT('',(2.635,4.4,4.5));
#3726=CARTESIAN_POINT('Origin',(2.8,4.4,4.5));
#3727=CARTESIAN_POINT('',(2.635,6.,4.5));
#3728=CARTESIAN_POINT('',(2.635,4.4,4.5));
#3729=CARTESIAN_POINT('Origin',(2.8,6.,4.5));
#3730=CARTESIAN_POINT('Origin',(2.8,4.4,4.5));
#3731=CARTESIAN_POINT('Origin',(-5.14351655641888E-16,4.4,1.7));
#3732=CARTESIAN_POINT('',(-0.165000000000001,4.4,1.7));
#3733=CARTESIAN_POINT('Origin',(-5.14351655641888E-16,4.4,1.7));
#3734=CARTESIAN_POINT('',(-0.165000000000001,6.,1.7));
#3735=CARTESIAN_POINT('',(-0.165000000000001,4.4,1.7));
#3736=CARTESIAN_POINT('Origin',(-5.14351655641888E-16,6.,1.7));
#3737=CARTESIAN_POINT('Origin',(-5.27355936696949E-16,4.4,1.7));
#3738=CARTESIAN_POINT('Origin',(-2.8,-0.1,4.5));
#3739=CARTESIAN_POINT('',(-2.965,0.,4.5));
#3740=CARTESIAN_POINT('Origin',(-2.8,0.,4.5));
#3741=CARTESIAN_POINT('',(-2.965,1.6,4.5));
#3742=CARTESIAN_POINT('',(-2.965,-0.1,4.5));
#3743=CARTESIAN_POINT('Origin',(-2.8,1.6,4.5));
#3744=CARTESIAN_POINT('Origin',(-2.8,1.6,4.5));
#3745=CARTESIAN_POINT('Origin',(1.71450551880629E-16,-0.1,7.3));
#3746=CARTESIAN_POINT('',(-0.165,0.,7.3));
#3747=CARTESIAN_POINT('Origin',(1.71450551880629E-16,0.,7.3));
#3748=CARTESIAN_POINT('',(-0.165,1.6,7.3));
#3749=CARTESIAN_POINT('',(-0.165,-0.1,7.3));
#3750=CARTESIAN_POINT('Origin',(1.71450551880629E-16,1.6,7.3));
#3751=CARTESIAN_POINT('Origin',(1.66533453693773E-16,1.6,7.3));
#3752=CARTESIAN_POINT('Origin',(2.8,-0.1,4.5));
#3753=CARTESIAN_POINT('',(2.635,0.,4.5));
#3754=CARTESIAN_POINT('Origin',(2.8,0.,4.5));
#3755=CARTESIAN_POINT('',(2.635,1.6,4.5));
#3756=CARTESIAN_POINT('',(2.635,-0.1,4.5));
#3757=CARTESIAN_POINT('Origin',(2.8,1.6,4.5));
#3758=CARTESIAN_POINT('Origin',(2.8,1.6,4.5));
#3759=CARTESIAN_POINT('Origin',(-5.14351655641888E-16,-0.1,1.7));
#3760=CARTESIAN_POINT('',(-0.165000000000001,0.,1.7));
#3761=CARTESIAN_POINT('Origin',(-5.14351655641888E-16,0.,1.7));
#3762=CARTESIAN_POINT('',(-0.165000000000001,1.6,1.7));
#3763=CARTESIAN_POINT('',(-0.165000000000001,-0.1,1.7));
#3764=CARTESIAN_POINT('Origin',(-5.14351655641888E-16,1.6,1.7));
#3765=CARTESIAN_POINT('Origin',(-5.27355936696949E-16,1.6,1.7));
#3766=CARTESIAN_POINT('Origin',(0.,2.8,4.5));
#3767=CARTESIAN_POINT('',(-5.,2.8,4.5));
#3768=CARTESIAN_POINT('Origin',(0.,2.8,4.5));
#3769=CARTESIAN_POINT('',(-3.5,2.8,4.5));
#3770=CARTESIAN_POINT('Origin',(0.,2.8,4.5));
#3771=CARTESIAN_POINT('Origin',(0.,2.,4.5));
#3772=CARTESIAN_POINT('',(-5.,2.,4.5));
#3773=CARTESIAN_POINT('Origin',(0.,2.,4.5));
#3774=CARTESIAN_POINT('',(-3.5,2.,4.5));
#3775=CARTESIAN_POINT('Origin',(0.,2.,4.5));
#3776=CARTESIAN_POINT('Origin',(0.,2.,4.5));
#3777=CARTESIAN_POINT('',(-5.,2.,4.5));
#3778=CARTESIAN_POINT('Origin',(0.,0.,4.5));
#3779=CARTESIAN_POINT('',(-3.5,0.,4.5));
#3780=CARTESIAN_POINT('',(-3.5,0.,4.5));
#3781=CARTESIAN_POINT('Origin',(0.,0.,4.5));
#3782=CARTESIAN_POINT('Origin',(0.,0.,4.5));
#3783=CARTESIAN_POINT('',(-2.35,6.,4.5));
#3784=CARTESIAN_POINT('Origin',(0.,6.,4.5));
#3785=CARTESIAN_POINT('',(-2.35,0.,4.5));
#3786=CARTESIAN_POINT('',(-2.35,0.,4.5));
#3787=CARTESIAN_POINT('Origin',(0.,0.,4.5));
#3788=CARTESIAN_POINT('Origin',(0.,0.,4.5));
#3789=CARTESIAN_POINT('',(-3.5,6.,4.5));
#3790=CARTESIAN_POINT('Origin',(0.,6.,4.5));
#3791=CARTESIAN_POINT('',(-3.5,0.,4.5));
#3792=CARTESIAN_POINT('Origin',(0.,6.,4.5));
#3793=CARTESIAN_POINT('Origin',(0.,0.,4.5));
#3794=CARTESIAN_POINT('',(0.,0.,0.));
#3795=CARTESIAN_POINT('',(0.,0.,0.));
#3796=CARTESIAN_POINT('Origin',(0.,0.,0.));
#3797=CARTESIAN_POINT('',(-1.63531,-0.410863395882378,-2.00267715711366E-16));
#3798=CARTESIAN_POINT('',(-2.00267715711366E-16,-0.410863395882378,1.63531));
#3799=CARTESIAN_POINT('Origin',(0.,-0.410863395882378,0.));
#3800=CARTESIAN_POINT('Origin',(0.,-0.410863395882378,0.));
#3801=CARTESIAN_POINT('',(-2.00267715711366E-16,0.410863395882378,1.63531));
#3802=CARTESIAN_POINT('Origin',(-2.05128338857182E-16,0.,1.675));
#3803=CARTESIAN_POINT('',(-1.63531,0.410863395882378,2.00267715711366E-16));
#3804=CARTESIAN_POINT('Origin',(0.,0.410863395882378,0.));
#3805=CARTESIAN_POINT('Origin',(0.,0.410863395882378,0.));
#3806=CARTESIAN_POINT('Origin',(0.,0.,0.));
#3807=CARTESIAN_POINT('',(-1.63531,0.7,-2.00267715711366E-16));
#3808=CARTESIAN_POINT('',(-1.63531,0.,-2.00267715711366E-16));
#3809=CARTESIAN_POINT('Origin',(0.,0.7,0.));
#3810=CARTESIAN_POINT('Origin',(0.,0.,0.));
#3811=CARTESIAN_POINT('',(-1.,-0.6,-1.22464679914735E-16));
#3812=CARTESIAN_POINT('Origin',(0.,-0.6,0.));
#3813=CARTESIAN_POINT('',(-1.,0.6,-1.22464679914735E-16));
#3814=CARTESIAN_POINT('',(-1.,0.,-1.22464679914735E-16));
#3815=CARTESIAN_POINT('Origin',(0.,0.6,0.));
#3816=CARTESIAN_POINT('Origin',(0.,0.65,0.));
#3817=CARTESIAN_POINT('',(-1.1,0.7,-1.34711147906209E-16));
#3818=CARTESIAN_POINT('',(-1.05,0.65,-1.28587913910472E-16));
#3819=CARTESIAN_POINT('Origin',(0.,0.7,0.));
#3820=CARTESIAN_POINT('Origin',(1.63531,0.7,0.));
#3821=CARTESIAN_POINT('Origin',(0.,0.,0.));
#3822=CARTESIAN_POINT('',(-1.63531,-0.7,-2.00267715711366E-16));
#3823=CARTESIAN_POINT('Origin',(0.,-0.7,0.));
#3824=CARTESIAN_POINT('',(-1.63531,0.,-2.00267715711366E-16));
#3825=CARTESIAN_POINT('Origin',(1.1,-0.7,0.));
#3826=CARTESIAN_POINT('',(-1.1,-0.7,-1.34711147906209E-16));
#3827=CARTESIAN_POINT('Origin',(0.,-0.7,0.));
#3828=CARTESIAN_POINT('Origin',(0.,-0.65,0.));
#3829=CARTESIAN_POINT('',(-1.05,-0.65,-1.28587913910472E-16));
#3830=CARTESIAN_POINT('',(0.,0.,0.));
#3831=CARTESIAN_POINT('Origin',(0.,0.,0.));
#3832=CARTESIAN_POINT('',(-1.71469,0.410863395882378,-2.09988962002998E-16));
#3833=CARTESIAN_POINT('',(-2.09988962002998E-16,0.410863395882378,1.71469));
#3834=CARTESIAN_POINT('Origin',(0.,0.410863395882378,0.));
#3835=CARTESIAN_POINT('Origin',(0.,0.410863395882378,0.));
#3836=CARTESIAN_POINT('',(-2.09988962002998E-16,-0.410863395882378,1.71469));
#3837=CARTESIAN_POINT('Origin',(-2.05128338857182E-16,0.,1.675));
#3838=CARTESIAN_POINT('',(-1.71469,-0.410863395882378,2.09988962002998E-16));
#3839=CARTESIAN_POINT('Origin',(0.,-0.410863395882378,0.));
#3840=CARTESIAN_POINT('Origin',(0.,-0.410863395882378,0.));
#3841=CARTESIAN_POINT('Origin',(0.,0.,0.));
#3842=CARTESIAN_POINT('',(-1.71469,-0.7,-2.09988962002998E-16));
#3843=CARTESIAN_POINT('Origin',(0.,-0.7,0.));
#3844=CARTESIAN_POINT('',(-1.71469,0.,-2.09988962002998E-16));
#3845=CARTESIAN_POINT('Origin',(2.25,0.7,0.));
#3846=CARTESIAN_POINT('',(-2.25,0.7,-2.75545529808154E-16));
#3847=CARTESIAN_POINT('Origin',(0.,0.7,0.));
#3848=CARTESIAN_POINT('',(-1.71469,0.7,-2.09988962002998E-16));
#3849=CARTESIAN_POINT('Origin',(0.,0.7,0.));
#3850=CARTESIAN_POINT('Origin',(0.,0.65,0.));
#3851=CARTESIAN_POINT('',(-2.35,0.6,-2.87791997799628E-16));
#3852=CARTESIAN_POINT('Origin',(0.,0.6,0.));
#3853=CARTESIAN_POINT('',(-2.3,0.65,-2.81668763803891E-16));
#3854=CARTESIAN_POINT('Origin',(0.,0.,0.));
#3855=CARTESIAN_POINT('',(-2.35,-0.6,-2.87791997799628E-16));
#3856=CARTESIAN_POINT('Origin',(0.,-0.6,0.));
#3857=CARTESIAN_POINT('',(-2.35,0.,-2.87791997799628E-16));
#3858=CARTESIAN_POINT('Origin',(0.,-0.65,0.));
#3859=CARTESIAN_POINT('',(-2.25,-0.7,-2.75545529808154E-16));
#3860=CARTESIAN_POINT('Origin',(0.,-0.7,0.));
#3861=CARTESIAN_POINT('',(-2.3,-0.65,-2.81668763803891E-16));
#3862=CARTESIAN_POINT('Origin',(1.71469,-0.7,0.));
#3863=CARTESIAN_POINT('Origin',(0.,0.,0.));
#3864=CARTESIAN_POINT('',(-1.71469,0.,-2.09988962002998E-16));
#3865=CARTESIAN_POINT('',(0.,0.,0.));
#3866=CARTESIAN_POINT('Origin',(1.675,0.,0.));
#3867=CARTESIAN_POINT('',(1.675,-2.97627328869245E-33,0.3969));
#3868=CARTESIAN_POINT('',(1.675,-2.97627328869245E-33,-0.3969));
#3869=CARTESIAN_POINT('Origin',(1.675,0.,0.));
#3870=CARTESIAN_POINT('Origin',(1.18440385848747,0.,-1.18440385848747));
#3871=CARTESIAN_POINT('',(1.46505453994041,3.1867025333467E-33,-0.903753177034526));
#3872=CARTESIAN_POINT('',(0.903753177034527,-9.13924911073161E-33,-1.46505453994041));
#3873=CARTESIAN_POINT('Origin',(1.18440385848747,0.,-1.18440385848747));
#3874=CARTESIAN_POINT('Origin',(1.02564169428591E-16,0.,-1.675));
#3875=CARTESIAN_POINT('',(0.3969,-2.97627328869246E-33,-1.675));
#3876=CARTESIAN_POINT('',(-0.3969,-2.97627328869245E-33,-1.675));
#3877=CARTESIAN_POINT('Origin',(1.02564169428591E-16,0.,-1.675));
#3878=CARTESIAN_POINT('Origin',(-1.18440385848747,0.,-1.18440385848747));
#3879=CARTESIAN_POINT('',(-0.903753177034526,3.1867025333467E-33,-1.46505453994041));
#3880=CARTESIAN_POINT('',(-1.46505453994041,-9.13924911073161E-33,-0.903753177034527));
#3881=CARTESIAN_POINT('Origin',(-1.18440385848747,0.,-1.18440385848747));
#3882=CARTESIAN_POINT('Origin',(-1.675,0.,-2.05128338857182E-16));
#3883=CARTESIAN_POINT('',(-1.675,-2.97627328869246E-33,-0.3969));
#3884=CARTESIAN_POINT('',(-1.675,-2.97627328869245E-33,0.3969));
#3885=CARTESIAN_POINT('Origin',(-1.675,0.,-2.05128338857182E-16));
#3886=CARTESIAN_POINT('Origin',(-1.18440385848747,0.,1.18440385848747));
#3887=CARTESIAN_POINT('',(-1.46505453994041,6.26819044436628E-33,0.903753177034526));
#3888=CARTESIAN_POINT('',(-0.903753177034527,-1.22207370217512E-32,1.46505453994041));
#3889=CARTESIAN_POINT('Origin',(-1.18440385848747,0.,1.18440385848747));
#3890=CARTESIAN_POINT('Origin',(-3.07692508285772E-16,0.,1.675));
#3891=CARTESIAN_POINT('',(-0.3969,-2.97627328869246E-33,1.675));
#3892=CARTESIAN_POINT('',(0.396899999999999,-2.97627328869245E-33,1.675));
#3893=CARTESIAN_POINT('Origin',(-3.07692508285772E-16,0.,1.675));
#3894=CARTESIAN_POINT('Origin',(1.18440385848747,0.,1.18440385848747));
#3895=CARTESIAN_POINT('',(0.903753177034526,9.34967835538585E-33,1.46505453994041));
#3896=CARTESIAN_POINT('',(1.46505453994041,-1.53022249327708E-32,0.903753177034527));
#3897=CARTESIAN_POINT('Origin',(1.18440385848747,0.,1.18440385848747));
#3898=CARTESIAN_POINT('',(0.,0.,0.));
#3899=CARTESIAN_POINT('Origin',(1.18440385848747,0.,1.18440385848747));
#3900=CARTESIAN_POINT('',(0.846804978391753,-0.07938,1.40825612658882));
#3901=CARTESIAN_POINT('',(1.40825612658882,-0.07938,0.846804978391754));
#3902=CARTESIAN_POINT('Ctrl Pts',(0.846804978391752,-0.0793800000000001,
1.40825612658882));
#3903=CARTESIAN_POINT('Ctrl Pts',(0.854205272175554,-0.123401821157026,
1.40380622184538));
#3904=CARTESIAN_POINT('Ctrl Pts',(0.867957148219441,-0.166543350814306,
1.39550172959303));
#3905=CARTESIAN_POINT('Ctrl Pts',(0.902193646979982,-0.237231147975234,
1.3735491215176));
#3906=CARTESIAN_POINT('Ctrl Pts',(0.920778333482564,-0.266264900654909,
1.36127834356734));
#3907=CARTESIAN_POINT('Ctrl Pts',(0.962485392528369,-0.317195968905306,
1.33211611256184));
#3908=CARTESIAN_POINT('Ctrl Pts',(0.985600426557816,-0.33909093068465,1.31521005565926));
#3909=CARTESIAN_POINT('Ctrl Pts',(1.03253285680459,-0.373586846396559,1.27866649102984));
#3910=CARTESIAN_POINT('Ctrl Pts',(1.05871835910697,-0.388086240756494,1.25722555095714));
#3911=CARTESIAN_POINT('Ctrl Pts',(1.11153475808518,-0.407068917407805,1.2107812086231));
#3912=CARTESIAN_POINT('Ctrl Pts',(1.13814686046673,-0.411552957311693,1.18575674747573));
#3913=CARTESIAN_POINT('Ctrl Pts',(1.18575674747573,-0.411552957311693,1.13814686046673));
#3914=CARTESIAN_POINT('Ctrl Pts',(1.2107812086231,-0.407068917407805,1.11153475808518));
#3915=CARTESIAN_POINT('Ctrl Pts',(1.25722555095713,-0.388086240756494,1.05871835910697));
#3916=CARTESIAN_POINT('Ctrl Pts',(1.27866649102984,-0.373586846396559,1.03253285680459));
#3917=CARTESIAN_POINT('Ctrl Pts',(1.31521005565926,-0.33909093068465,0.985600426557816));
#3918=CARTESIAN_POINT('Ctrl Pts',(1.33211611256184,-0.317195968905306,0.962485392528369));
#3919=CARTESIAN_POINT('Ctrl Pts',(1.36127834356734,-0.266264900654909,0.920778333482565));
#3920=CARTESIAN_POINT('Ctrl Pts',(1.3735491215176,-0.237231147975234,0.902193646979983));
#3921=CARTESIAN_POINT('Ctrl Pts',(1.39550172959303,-0.166543350814306,0.867957148219442));
#3922=CARTESIAN_POINT('Ctrl Pts',(1.40380622184538,-0.123401821157026,0.854205272175555));
#3923=CARTESIAN_POINT('Ctrl Pts',(1.40825612658882,-0.0793800000000001,
0.846804978391753));
#3924=CARTESIAN_POINT('',(0.886256117232623,-0.07938,1.45861320581289));
#3925=CARTESIAN_POINT('Origin',(1.18440385848747,-0.07938,1.18440385848747));
#3926=CARTESIAN_POINT('',(1.45861320581289,-0.07938,0.886256117232624));
#3927=CARTESIAN_POINT('Ctrl Pts',(1.45861320581289,-0.0793800000000001,
0.886256117232623));
#3928=CARTESIAN_POINT('Ctrl Pts',(1.45630208793976,-0.101649918886749,0.890059788636852));
#3929=CARTESIAN_POINT('Ctrl Pts',(1.45296717977858,-0.123823518623746,0.895520212222107));
#3930=CARTESIAN_POINT('Ctrl Pts',(1.43904931717599,-0.192480977588836,0.917859913453975));
#3931=CARTESIAN_POINT('Ctrl Pts',(1.4243271592157,-0.236152929235938,0.940896403863072));
#3932=CARTESIAN_POINT('Ctrl Pts',(1.39055359345152,-0.303141259068212,0.990027513266106));
#3933=CARTESIAN_POINT('Ctrl Pts',(1.36743459453896,-0.335108247315849,1.02199477007745));
#3934=CARTESIAN_POINT('Ctrl Pts',(1.32643091652006,-0.373243761060364,1.07446535104584));
#3935=CARTESIAN_POINT('Ctrl Pts',(1.30441816675528,-0.387888272594439,1.10126842659597));
#3936=CARTESIAN_POINT('Ctrl Pts',(1.25681160160691,-0.407041111792943,1.15530234155453));
#3937=CARTESIAN_POINT('Ctrl Pts',(1.23119764287622,-0.411552957311693,1.18251418313119));
#3938=CARTESIAN_POINT('Ctrl Pts',(1.18251418313119,-0.411552957311693,1.23119764287622));
#3939=CARTESIAN_POINT('Ctrl Pts',(1.15530234155453,-0.407041111792943,1.25681160160691));
#3940=CARTESIAN_POINT('Ctrl Pts',(1.10126842659597,-0.387888272594439,1.30441816675528));
#3941=CARTESIAN_POINT('Ctrl Pts',(1.07446535104584,-0.373243761060364,1.32643091652006));
#3942=CARTESIAN_POINT('Ctrl Pts',(1.02199477007745,-0.335108247315848,1.36743459453896));
#3943=CARTESIAN_POINT('Ctrl Pts',(0.990027513266105,-0.303141259068211,
1.39055359345152));
#3944=CARTESIAN_POINT('Ctrl Pts',(0.940896403863071,-0.236152929235937,
1.42432715921571));
#3945=CARTESIAN_POINT('Ctrl Pts',(0.917859913453974,-0.192480977588835,
1.43904931717599));
#3946=CARTESIAN_POINT('Ctrl Pts',(0.895520212222106,-0.123823518623745,
1.45296717977858));
#3947=CARTESIAN_POINT('Ctrl Pts',(0.890059788636851,-0.101649918886749,
1.45630208793976));
#3948=CARTESIAN_POINT('Ctrl Pts',(0.886256117232622,-0.0793800000000001,
1.45861320581289));
#3949=CARTESIAN_POINT('Origin',(1.18440385848747,-0.07938,1.18440385848747));
#3950=CARTESIAN_POINT('Origin',(0.,-0.27783,0.));
#3951=CARTESIAN_POINT('',(0.404717578595295,-0.07938,1.65807299932179));
#3952=CARTESIAN_POINT('Origin',(0.,-0.07938,0.));
#3953=CARTESIAN_POINT('',(-0.404717578595296,-0.07938,1.65807299932179));
#3954=CARTESIAN_POINT('Ctrl Pts',(0.404717578595296,-0.0793800000000001,
1.65807299932179));
#3955=CARTESIAN_POINT('Ctrl Pts',(0.400393769631747,-0.101649918886749,
1.65912839404491));
#3956=CARTESIAN_POINT('Ctrl Pts',(0.394174530911058,-0.123823518623745,
1.66063136041479));
#3957=CARTESIAN_POINT('Ctrl Pts',(0.368536561654407,-0.192480977588835,
1.66658649961961));
#3958=CARTESIAN_POINT('Ctrl Pts',(0.341837165343982,-0.236152929235937,
1.67246562047521));
#3959=CARTESIAN_POINT('Ctrl Pts',(0.283214707341173,-0.303141259068211,
1.68332504372461));
#3960=CARTESIAN_POINT('Ctrl Pts',(0.244262842368623,-0.335108247315849,
1.68958170688653));
#3961=CARTESIAN_POINT('Ctrl Pts',(0.178166559972324,-0.373243761060364,
1.69769003172132));
#3962=CARTESIAN_POINT('Ctrl Pts',(0.143648558862931,-0.387888272594439,
1.70107730356824));
#3963=CARTESIAN_POINT('Ctrl Pts',(0.0717778861362652,-0.407041111792943,
1.70562212620408));
#3964=CARTESIAN_POINT('Ctrl Pts',(0.0344244045173309,-0.411552957311693,
1.706752));
#3965=CARTESIAN_POINT('Ctrl Pts',(-0.0344244045173315,-0.411552957311693,
1.706752));
#3966=CARTESIAN_POINT('Ctrl Pts',(-0.0717778861362658,-0.407041111792943,
1.70562212620408));
#3967=CARTESIAN_POINT('Ctrl Pts',(-0.143648558862932,-0.387888272594439,
1.70107730356824));
#3968=CARTESIAN_POINT('Ctrl Pts',(-0.178166559972325,-0.373243761060364,
1.69769003172132));
#3969=CARTESIAN_POINT('Ctrl Pts',(-0.244262842368624,-0.335108247315849,
1.68958170688653));
#3970=CARTESIAN_POINT('Ctrl Pts',(-0.283214707341173,-0.303141259068212,
1.68332504372461));
#3971=CARTESIAN_POINT('Ctrl Pts',(-0.341837165343982,-0.236152929235937,
1.67246562047521));
#3972=CARTESIAN_POINT('Ctrl Pts',(-0.368536561654408,-0.192480977588835,
1.66658649961961));
#3973=CARTESIAN_POINT('Ctrl Pts',(-0.394174530911059,-0.123823518623745,
1.66063136041479));
#3974=CARTESIAN_POINT('Ctrl Pts',(-0.400393769631748,-0.101649918886749,
1.65912839404491));
#3975=CARTESIAN_POINT('Ctrl Pts',(-0.404717578595297,-0.0793800000000001,
1.65807299932179));
#3976=CARTESIAN_POINT('',(-0.886256117232624,-0.07938,1.45861320581289));
#3977=CARTESIAN_POINT('Origin',(0.,-0.07938,0.));
#3978=CARTESIAN_POINT('',(-1.45861320581289,-0.07938,0.886256117232623));
#3979=CARTESIAN_POINT('Ctrl Pts',(-0.886256117232623,-0.0793800000000001,
1.45861320581289));
#3980=CARTESIAN_POINT('Ctrl Pts',(-0.890059788636852,-0.101649918886749,
1.45630208793976));
#3981=CARTESIAN_POINT('Ctrl Pts',(-0.895520212222106,-0.123823518623745,
1.45296717977858));
#3982=CARTESIAN_POINT('Ctrl Pts',(-0.917859913453974,-0.192480977588835,
1.43904931717599));
#3983=CARTESIAN_POINT('Ctrl Pts',(-0.940896403863071,-0.236152929235937,
1.4243271592157));
#3984=CARTESIAN_POINT('Ctrl Pts',(-0.990027513266105,-0.303141259068211,
1.39055359345152));
#3985=CARTESIAN_POINT('Ctrl Pts',(-1.02199477007745,-0.335108247315848,
1.36743459453896));
#3986=CARTESIAN_POINT('Ctrl Pts',(-1.07446535104584,-0.373243761060364,
1.32643091652006));
#3987=CARTESIAN_POINT('Ctrl Pts',(-1.10126842659597,-0.387888272594439,
1.30441816675528));
#3988=CARTESIAN_POINT('Ctrl Pts',(-1.15530234155453,-0.407041111792943,
1.25681160160691));
#3989=CARTESIAN_POINT('Ctrl Pts',(-1.18251418313119,-0.411552957311693,
1.23119764287622));
#3990=CARTESIAN_POINT('Ctrl Pts',(-1.23119764287622,-0.411552957311693,
1.18251418313119));
#3991=CARTESIAN_POINT('Ctrl Pts',(-1.25681160160691,-0.407041111792943,
1.15530234155453));
#3992=CARTESIAN_POINT('Ctrl Pts',(-1.30441816675528,-0.387888272594439,
1.10126842659597));
#3993=CARTESIAN_POINT('Ctrl Pts',(-1.32643091652006,-0.373243761060365,
1.07446535104584));
#3994=CARTESIAN_POINT('Ctrl Pts',(-1.36743459453896,-0.335108247315849,
1.02199477007745));
#3995=CARTESIAN_POINT('Ctrl Pts',(-1.39055359345152,-0.303141259068212,
0.990027513266106));
#3996=CARTESIAN_POINT('Ctrl Pts',(-1.4243271592157,-0.236152929235938,0.940896403863071));
#3997=CARTESIAN_POINT('Ctrl Pts',(-1.43904931717599,-0.192480977588836,
0.917859913453974));
#3998=CARTESIAN_POINT('Ctrl Pts',(-1.45296717977858,-0.123823518623746,
0.895520212222106));
#3999=CARTESIAN_POINT('Ctrl Pts',(-1.45630208793976,-0.101649918886749,
0.890059788636852));
#4000=CARTESIAN_POINT('Ctrl Pts',(-1.45861320581289,-0.0793800000000001,
0.886256117232623));
#4001=CARTESIAN_POINT('',(-1.65807299932179,-0.07938,0.404717578595295));
#4002=CARTESIAN_POINT('Origin',(0.,-0.07938,0.));
#4003=CARTESIAN_POINT('',(-1.706752,-0.411552957311693,2.08591827245526E-16));
#4004=CARTESIAN_POINT('Ctrl Pts',(-1.65807299932179,-0.0793800000000001,
0.404717578595296));
#4005=CARTESIAN_POINT('Ctrl Pts',(-1.65912839404491,-0.101649918886749,
0.400393769631747));
#4006=CARTESIAN_POINT('Ctrl Pts',(-1.66063136041479,-0.123823518623745,
0.394174530911058));
#4007=CARTESIAN_POINT('Ctrl Pts',(-1.66658649961961,-0.192480977588835,
0.368536561654407));
#4008=CARTESIAN_POINT('Ctrl Pts',(-1.67246562047521,-0.236152929235937,
0.341837165343982));
#4009=CARTESIAN_POINT('Ctrl Pts',(-1.68332504372461,-0.303141259068211,
0.283214707341173));
#4010=CARTESIAN_POINT('Ctrl Pts',(-1.68958170688653,-0.335108247315848,
0.244262842368623));
#4011=CARTESIAN_POINT('Ctrl Pts',(-1.69769003172132,-0.373243761060364,
0.178166559972324));
#4012=CARTESIAN_POINT('Ctrl Pts',(-1.70107730356824,-0.387888272594439,
0.143648558862931));
#4013=CARTESIAN_POINT('Ctrl Pts',(-1.70562212620408,-0.407041111792943,
0.0717778861362656));
#4014=CARTESIAN_POINT('Ctrl Pts',(-1.706752,-0.411552957311693,0.0344244045173313));
#4015=CARTESIAN_POINT('Ctrl Pts',(-1.706752,-0.411552957311693,2.08166817117217E-16));
#4016=CARTESIAN_POINT('',(-1.706752,-0.47628,2.09016837373834E-16));
#4017=CARTESIAN_POINT('',(-1.706752,-0.27783,2.09016837373834E-16));
#4018=CARTESIAN_POINT('Origin',(0.,-0.47628,0.));
#4019=CARTESIAN_POINT('',(-1.65807299932179,-0.07938,-0.404717578595296));
#4020=CARTESIAN_POINT('Ctrl Pts',(-1.706752,-0.411552957311693,2.0122792321331E-16));
#4021=CARTESIAN_POINT('Ctrl Pts',(-1.706752,-0.411552957311693,-0.0344244045173309));
#4022=CARTESIAN_POINT('Ctrl Pts',(-1.70562212620408,-0.407041111792943,
-0.0717778861362652));
#4023=CARTESIAN_POINT('Ctrl Pts',(-1.70107730356824,-0.387888272594439,
-0.143648558862931));
#4024=CARTESIAN_POINT('Ctrl Pts',(-1.69769003172132,-0.373243761060365,
-0.178166559972324));
#4025=CARTESIAN_POINT('Ctrl Pts',(-1.68958170688653,-0.335108247315849,
-0.244262842368623));
#4026=CARTESIAN_POINT('Ctrl Pts',(-1.68332504372461,-0.303141259068212,
-0.283214707341173));
#4027=CARTESIAN_POINT('Ctrl Pts',(-1.67246562047521,-0.236152929235938,
-0.341837165343982));
#4028=CARTESIAN_POINT('Ctrl Pts',(-1.66658649961961,-0.192480977588836,
-0.368536561654407));
#4029=CARTESIAN_POINT('Ctrl Pts',(-1.66063136041479,-0.123823518623745,
-0.394174530911059));
#4030=CARTESIAN_POINT('Ctrl Pts',(-1.65912839404491,-0.101649918886749,
-0.400393769631748));
#4031=CARTESIAN_POINT('Ctrl Pts',(-1.65807299932179,-0.0793800000000001,
-0.404717578595296));
#4032=CARTESIAN_POINT('',(-1.45861320581289,-0.07938,-0.886256117232623));
#4033=CARTESIAN_POINT('Origin',(0.,-0.07938,0.));
#4034=CARTESIAN_POINT('',(-0.886256117232623,-0.07938,-1.45861320581289));
#4035=CARTESIAN_POINT('Ctrl Pts',(-1.45861320581289,-0.0793800000000001,
-0.886256117232623));
#4036=CARTESIAN_POINT('Ctrl Pts',(-1.45630208793976,-0.101649918886749,
-0.890059788636852));
#4037=CARTESIAN_POINT('Ctrl Pts',(-1.45296717977858,-0.123823518623745,
-0.895520212222106));
#4038=CARTESIAN_POINT('Ctrl Pts',(-1.43904931717599,-0.192480977588835,
-0.917859913453974));
#4039=CARTESIAN_POINT('Ctrl Pts',(-1.4243271592157,-0.236152929235937,-0.940896403863072));
#4040=CARTESIAN_POINT('Ctrl Pts',(-1.39055359345152,-0.303141259068212,
-0.990027513266106));
#4041=CARTESIAN_POINT('Ctrl Pts',(-1.36743459453896,-0.335108247315849,
-1.02199477007745));
#4042=CARTESIAN_POINT('Ctrl Pts',(-1.32643091652006,-0.373243761060364,
-1.07446535104584));
#4043=CARTESIAN_POINT('Ctrl Pts',(-1.30441816675528,-0.387888272594439,
-1.10126842659597));
#4044=CARTESIAN_POINT('Ctrl Pts',(-1.25681160160691,-0.407041111792943,
-1.15530234155453));
#4045=CARTESIAN_POINT('Ctrl Pts',(-1.23119764287622,-0.411552957311693,
-1.18251418313119));
#4046=CARTESIAN_POINT('Ctrl Pts',(-1.18251418313119,-0.411552957311693,
-1.23119764287622));
#4047=CARTESIAN_POINT('Ctrl Pts',(-1.15530234155453,-0.407041111792943,
-1.25681160160691));
#4048=CARTESIAN_POINT('Ctrl Pts',(-1.10126842659597,-0.387888272594439,
-1.30441816675528));
#4049=CARTESIAN_POINT('Ctrl Pts',(-1.07446535104584,-0.373243761060364,
-1.32643091652006));
#4050=CARTESIAN_POINT('Ctrl Pts',(-1.02199477007745,-0.335108247315848,
-1.36743459453896));
#4051=CARTESIAN_POINT('Ctrl Pts',(-0.990027513266105,-0.303141259068211,
-1.39055359345152));
#4052=CARTESIAN_POINT('Ctrl Pts',(-0.940896403863071,-0.236152929235936,
-1.42432715921571));
#4053=CARTESIAN_POINT('Ctrl Pts',(-0.917859913453974,-0.192480977588835,
-1.43904931717599));
#4054=CARTESIAN_POINT('Ctrl Pts',(-0.895520212222106,-0.123823518623745,
-1.45296717977858));
#4055=CARTESIAN_POINT('Ctrl Pts',(-0.890059788636851,-0.101649918886749,
-1.45630208793976));
#4056=CARTESIAN_POINT('Ctrl Pts',(-0.886256117232623,-0.0793800000000001,
-1.45861320581289));
#4057=CARTESIAN_POINT('',(-0.404717578595295,-0.07938,-1.65807299932179));
#4058=CARTESIAN_POINT('Origin',(0.,-0.07938,0.));
#4059=CARTESIAN_POINT('',(0.404717578595296,-0.07938,-1.65807299932179));
#4060=CARTESIAN_POINT('Ctrl Pts',(-0.404717578595296,-0.0793800000000001,
-1.65807299932179));
#4061=CARTESIAN_POINT('Ctrl Pts',(-0.400393769631747,-0.101649918886749,
-1.65912839404491));
#4062=CARTESIAN_POINT('Ctrl Pts',(-0.394174530911058,-0.123823518623746,
-1.66063136041479));
#4063=CARTESIAN_POINT('Ctrl Pts',(-0.368536561654407,-0.192480977588836,
-1.66658649961961));
#4064=CARTESIAN_POINT('Ctrl Pts',(-0.341837165343982,-0.236152929235938,
-1.67246562047521));
#4065=CARTESIAN_POINT('Ctrl Pts',(-0.283214707341173,-0.303141259068212,
-1.68332504372461));
#4066=CARTESIAN_POINT('Ctrl Pts',(-0.244262842368623,-0.335108247315849,
-1.68958170688653));
#4067=CARTESIAN_POINT('Ctrl Pts',(-0.178166559972324,-0.373243761060364,
-1.69769003172132));
#4068=CARTESIAN_POINT('Ctrl Pts',(-0.143648558862931,-0.387888272594439,
-1.70107730356824));
#4069=CARTESIAN_POINT('Ctrl Pts',(-0.0717778861362653,-0.407041111792943,
-1.70562212620408));
#4070=CARTESIAN_POINT('Ctrl Pts',(-0.034424404517331,-0.411552957311693,
-1.706752));
#4071=CARTESIAN_POINT('Ctrl Pts',(0.0344244045173312,-0.411552957311693,
-1.706752));
#4072=CARTESIAN_POINT('Ctrl Pts',(0.0717778861362655,-0.407041111792943,
-1.70562212620408));
#4073=CARTESIAN_POINT('Ctrl Pts',(0.143648558862931,-0.387888272594439,
-1.70107730356824));
#4074=CARTESIAN_POINT('Ctrl Pts',(0.178166559972324,-0.373243761060364,
-1.69769003172132));
#4075=CARTESIAN_POINT('Ctrl Pts',(0.244262842368623,-0.335108247315849,
-1.68958170688653));
#4076=CARTESIAN_POINT('Ctrl Pts',(0.283214707341173,-0.303141259068212,
-1.68332504372461));
#4077=CARTESIAN_POINT('Ctrl Pts',(0.341837165343982,-0.236152929235937,
-1.67246562047521));
#4078=CARTESIAN_POINT('Ctrl Pts',(0.368536561654407,-0.192480977588835,
-1.66658649961961));
#4079=CARTESIAN_POINT('Ctrl Pts',(0.394174530911059,-0.123823518623745,
-1.66063136041479));
#4080=CARTESIAN_POINT('Ctrl Pts',(0.400393769631748,-0.101649918886749,
-1.65912839404491));
#4081=CARTESIAN_POINT('Ctrl Pts',(0.404717578595296,-0.0793800000000001,
-1.65807299932179));
#4082=CARTESIAN_POINT('',(0.886256117232623,-0.07938,-1.45861320581289));
#4083=CARTESIAN_POINT('Origin',(0.,-0.07938,0.));
#4084=CARTESIAN_POINT('',(1.45861320581289,-0.07938,-0.886256117232623));
#4085=CARTESIAN_POINT('Ctrl Pts',(0.886256117232623,-0.0793800000000001,
-1.45861320581289));
#4086=CARTESIAN_POINT('Ctrl Pts',(0.890059788636852,-0.101649918886749,
-1.45630208793976));
#4087=CARTESIAN_POINT('Ctrl Pts',(0.895520212222106,-0.123823518623745,
-1.45296717977858));
#4088=CARTESIAN_POINT('Ctrl Pts',(0.917859913453974,-0.192480977588835,
-1.43904931717599));
#4089=CARTESIAN_POINT('Ctrl Pts',(0.940896403863072,-0.236152929235937,
-1.4243271592157));
#4090=CARTESIAN_POINT('Ctrl Pts',(0.990027513266106,-0.303141259068211,
-1.39055359345152));
#4091=CARTESIAN_POINT('Ctrl Pts',(1.02199477007745,-0.335108247315849,-1.36743459453896));
#4092=CARTESIAN_POINT('Ctrl Pts',(1.07446535104584,-0.373243761060364,-1.32643091652006));
#4093=CARTESIAN_POINT('Ctrl Pts',(1.10126842659597,-0.387888272594439,-1.30441816675528));
#4094=CARTESIAN_POINT('Ctrl Pts',(1.15530234155453,-0.407041111792943,-1.25681160160691));
#4095=CARTESIAN_POINT('Ctrl Pts',(1.18251418313119,-0.411552957311693,-1.23119764287622));
#4096=CARTESIAN_POINT('Ctrl Pts',(1.23119764287622,-0.411552957311693,-1.18251418313119));
#4097=CARTESIAN_POINT('Ctrl Pts',(1.25681160160691,-0.407041111792943,-1.15530234155453));
#4098=CARTESIAN_POINT('Ctrl Pts',(1.30441816675528,-0.387888272594439,-1.10126842659597));
#4099=CARTESIAN_POINT('Ctrl Pts',(1.32643091652006,-0.373243761060364,-1.07446535104584));
#4100=CARTESIAN_POINT('Ctrl Pts',(1.36743459453896,-0.335108247315849,-1.02199477007745));
#4101=CARTESIAN_POINT('Ctrl Pts',(1.39055359345152,-0.303141259068212,-0.990027513266105));
#4102=CARTESIAN_POINT('Ctrl Pts',(1.4243271592157,-0.236152929235937,-0.940896403863071));
#4103=CARTESIAN_POINT('Ctrl Pts',(1.43904931717599,-0.192480977588835,-0.917859913453974));
#4104=CARTESIAN_POINT('Ctrl Pts',(1.45296717977858,-0.123823518623745,-0.895520212222106));
#4105=CARTESIAN_POINT('Ctrl Pts',(1.45630208793976,-0.101649918886749,-0.890059788636852));
#4106=CARTESIAN_POINT('Ctrl Pts',(1.45861320581289,-0.0793800000000001,
-0.886256117232623));
#4107=CARTESIAN_POINT('',(1.65807299932179,-0.07938,-0.404717578595296));
#4108=CARTESIAN_POINT('Origin',(0.,-0.07938,0.));
#4109=CARTESIAN_POINT('',(1.65807299932179,-0.07938,0.404717578595296));
#4110=CARTESIAN_POINT('Ctrl Pts',(1.65807299932179,-0.0793800000000001,
-0.404717578595296));
#4111=CARTESIAN_POINT('Ctrl Pts',(1.65912839404491,-0.101649918886749,-0.400393769631747));
#4112=CARTESIAN_POINT('Ctrl Pts',(1.66063136041479,-0.123823518623745,-0.394174530911058));
#4113=CARTESIAN_POINT('Ctrl Pts',(1.66658649961961,-0.192480977588835,-0.368536561654407));
#4114=CARTESIAN_POINT('Ctrl Pts',(1.67246562047521,-0.236152929235937,-0.341837165343982));
#4115=CARTESIAN_POINT('Ctrl Pts',(1.68332504372461,-0.303141259068212,-0.283214707341173));
#4116=CARTESIAN_POINT('Ctrl Pts',(1.68958170688653,-0.335108247315849,-0.244262842368623));
#4117=CARTESIAN_POINT('Ctrl Pts',(1.69769003172132,-0.373243761060364,-0.178166559972324));
#4118=CARTESIAN_POINT('Ctrl Pts',(1.70107730356824,-0.387888272594439,-0.143648558862931));
#4119=CARTESIAN_POINT('Ctrl Pts',(1.70562212620408,-0.407041111792943,-0.0717778861362655));
#4120=CARTESIAN_POINT('Ctrl Pts',(1.706752,-0.411552957311693,-0.0344244045173312));
#4121=CARTESIAN_POINT('Ctrl Pts',(1.706752,-0.411552957311693,0.0344244045173312));
#4122=CARTESIAN_POINT('Ctrl Pts',(1.70562212620408,-0.407041111792943,0.0717778861362655));
#4123=CARTESIAN_POINT('Ctrl Pts',(1.70107730356824,-0.387888272594439,0.143648558862931));
#4124=CARTESIAN_POINT('Ctrl Pts',(1.69769003172132,-0.373243761060364,0.178166559972324));
#4125=CARTESIAN_POINT('Ctrl Pts',(1.68958170688653,-0.335108247315849,0.244262842368623));
#4126=CARTESIAN_POINT('Ctrl Pts',(1.68332504372461,-0.303141259068212,0.283214707341173));
#4127=CARTESIAN_POINT('Ctrl Pts',(1.67246562047521,-0.236152929235937,0.341837165343982));
#4128=CARTESIAN_POINT('Ctrl Pts',(1.66658649961961,-0.192480977588835,0.368536561654407));
#4129=CARTESIAN_POINT('Ctrl Pts',(1.66063136041479,-0.123823518623745,0.394174530911058));
#4130=CARTESIAN_POINT('Ctrl Pts',(1.65912839404491,-0.101649918886749,0.400393769631747));
#4131=CARTESIAN_POINT('Ctrl Pts',(1.65807299932179,-0.0793800000000001,
0.404717578595296));
#4132=CARTESIAN_POINT('Origin',(0.,-0.07938,0.));
#4133=CARTESIAN_POINT('Origin',(0.,-0.07938,0.));
#4134=CARTESIAN_POINT('',(0.397005914195118,-0.07938,1.59456899932179));
#4135=CARTESIAN_POINT('Origin',(0.,-0.07938,0.));
#4136=CARTESIAN_POINT('Origin',(-3.33066907387547E-16,-0.07938,1.675));
#4137=CARTESIAN_POINT('Origin',(-3.33066907387547E-16,0.,1.675));
#4138=CARTESIAN_POINT('',(-0.397005914195118,-0.07938,1.59456899932179));
#4139=CARTESIAN_POINT('Ctrl Pts',(-0.397005914195119,-0.0793800000000001,
1.59456899932179));
#4140=CARTESIAN_POINT('Ctrl Pts',(-0.3886265584581,-0.123401821157026,1.59665523941937));
#4141=CARTESIAN_POINT('Ctrl Pts',(-0.373030350867485,-0.166543350814306,
1.60050712143809));
#4142=CARTESIAN_POINT('Ctrl Pts',(-0.333298652394954,-0.237231147975234,
1.60919314384089));
#4143=CARTESIAN_POINT('Ctrl Pts',(-0.311480544243687,-0.266264900654909,
1.61365775139403));
#4144=CARTESIAN_POINT('Ctrl Pts',(-0.261368388670537,-0.317195968905306,
1.62252828437015));
#4145=CARTESIAN_POINT('Ctrl Pts',(-0.233069203882014,-0.33909093068465,
1.62691869420078));
#4146=CARTESIAN_POINT('Ctrl Pts',(-0.174042761838764,-0.373586846396559,
1.63426473152765));
#4147=CARTESIAN_POINT('Ctrl Pts',(-0.14036578147155,-0.388086240756494,
1.63761964365402));
#4148=CARTESIAN_POINT('Ctrl Pts',(-0.0701778381840615,-0.407068917407805,
1.64212536811722));
#4149=CARTESIAN_POINT('Ctrl Pts',(-0.0336652739555918,-0.411552957311693,
1.643248));
#4150=CARTESIAN_POINT('Ctrl Pts',(0.0336652739555913,-0.411552957311693,
1.643248));
#4151=CARTESIAN_POINT('Ctrl Pts',(0.070177838184061,-0.407068917407805,
1.64212536811722));
#4152=CARTESIAN_POINT('Ctrl Pts',(0.140365781471549,-0.388086240756494,
1.63761964365402));
#4153=CARTESIAN_POINT('Ctrl Pts',(0.174042761838763,-0.373586846396559,
1.63426473152765));
#4154=CARTESIAN_POINT('Ctrl Pts',(0.233069203882014,-0.33909093068465,1.62691869420078));
#4155=CARTESIAN_POINT('Ctrl Pts',(0.261368388670536,-0.317195968905306,
1.62252828437015));
#4156=CARTESIAN_POINT('Ctrl Pts',(0.311480544243686,-0.266264900654908,
1.61365775139403));
#4157=CARTESIAN_POINT('Ctrl Pts',(0.333298652394954,-0.237231147975234,
1.60919314384089));
#4158=CARTESIAN_POINT('Ctrl Pts',(0.373030350867484,-0.166543350814306,
1.60050712143809));
#4159=CARTESIAN_POINT('Ctrl Pts',(0.388626558458099,-0.123401821157026,
1.59665523941937));
#4160=CARTESIAN_POINT('Ctrl Pts',(0.397005914195118,-0.07938,1.59456899932179));
#4161=CARTESIAN_POINT('Origin',(-3.33066907387547E-16,-0.07938,1.675));
#4162=CARTESIAN_POINT('Origin',(0.,-0.07938,0.));
#4163=CARTESIAN_POINT('',(-0.846804978391754,-0.07938,1.40825612658882));
#4164=CARTESIAN_POINT('Origin',(0.,-0.07938,0.));
#4165=CARTESIAN_POINT('Origin',(-1.18440385848747,-0.07938,1.18440385848747));
#4166=CARTESIAN_POINT('Origin',(-1.18440385848747,0.,1.18440385848747));
#4167=CARTESIAN_POINT('',(-1.40825612658882,-0.07938,0.846804978391753));
#4168=CARTESIAN_POINT('Ctrl Pts',(-1.40825612658882,-0.0793800000000001,
0.846804978391753));
#4169=CARTESIAN_POINT('Ctrl Pts',(-1.40380622184538,-0.123401821157026,
0.854205272175555));
#4170=CARTESIAN_POINT('Ctrl Pts',(-1.39550172959303,-0.166543350814306,
0.867957148219442));
#4171=CARTESIAN_POINT('Ctrl Pts',(-1.3735491215176,-0.237231147975235,0.902193646979983));
#4172=CARTESIAN_POINT('Ctrl Pts',(-1.36127834356734,-0.266264900654909,
0.920778333482565));
#4173=CARTESIAN_POINT('Ctrl Pts',(-1.33211611256184,-0.317195968905306,
0.962485392528369));
#4174=CARTESIAN_POINT('Ctrl Pts',(-1.31521005565926,-0.339090930684651,
0.985600426557816));
#4175=CARTESIAN_POINT('Ctrl Pts',(-1.27866649102984,-0.373586846396559,
1.03253285680459));
#4176=CARTESIAN_POINT('Ctrl Pts',(-1.25722555095714,-0.388086240756494,
1.05871835910697));
#4177=CARTESIAN_POINT('Ctrl Pts',(-1.2107812086231,-0.407068917407805,1.11153475808518));
#4178=CARTESIAN_POINT('Ctrl Pts',(-1.18575674747573,-0.411552957311693,
1.13814686046673));
#4179=CARTESIAN_POINT('Ctrl Pts',(-1.13814686046673,-0.411552957311693,
1.18575674747573));
#4180=CARTESIAN_POINT('Ctrl Pts',(-1.11153475808518,-0.407068917407805,
1.2107812086231));
#4181=CARTESIAN_POINT('Ctrl Pts',(-1.05871835910697,-0.388086240756494,
1.25722555095714));
#4182=CARTESIAN_POINT('Ctrl Pts',(-1.03253285680459,-0.373586846396559,
1.27866649102984));
#4183=CARTESIAN_POINT('Ctrl Pts',(-0.985600426557816,-0.33909093068465,
1.31521005565926));
#4184=CARTESIAN_POINT('Ctrl Pts',(-0.962485392528369,-0.317195968905306,
1.33211611256184));
#4185=CARTESIAN_POINT('Ctrl Pts',(-0.920778333482565,-0.266264900654908,
1.36127834356734));
#4186=CARTESIAN_POINT('Ctrl Pts',(-0.902193646979983,-0.237231147975234,
1.3735491215176));
#4187=CARTESIAN_POINT('Ctrl Pts',(-0.867957148219442,-0.166543350814306,
1.39550172959303));
#4188=CARTESIAN_POINT('Ctrl Pts',(-0.854205272175555,-0.123401821157026,
1.40380622184538));
#4189=CARTESIAN_POINT('Ctrl Pts',(-0.846804978391753,-0.0793800000000001,
1.40825612658882));
#4190=CARTESIAN_POINT('Origin',(-1.18440385848747,-0.07938,1.18440385848747));
#4191=CARTESIAN_POINT('Origin',(0.,-0.07938,0.));
#4192=CARTESIAN_POINT('',(-1.59456899932179,-0.07938,0.397005914195118));
#4193=CARTESIAN_POINT('Origin',(0.,-0.07938,0.));
#4194=CARTESIAN_POINT('Origin',(-1.675,-0.07938,-2.22044604925031E-16));
#4195=CARTESIAN_POINT('Origin',(-1.675,0.,-2.22044604925031E-16));
#4196=CARTESIAN_POINT('',(-1.59456899932179,-0.07938,-0.397005914195118));
#4197=CARTESIAN_POINT('',(-1.643248,-0.411552957311693,3.47540551556327E-18));
#4198=CARTESIAN_POINT('Ctrl Pts',(-1.59456899932179,-0.0793800000000001,
-0.397005914195119));
#4199=CARTESIAN_POINT('Ctrl Pts',(-1.59665523941937,-0.123401821157026,
-0.388626558458099));
#4200=CARTESIAN_POINT('Ctrl Pts',(-1.60050712143809,-0.166543350814306,
-0.373030350867485));
#4201=CARTESIAN_POINT('Ctrl Pts',(-1.60919314384089,-0.237231147975234,
-0.333298652394954));
#4202=CARTESIAN_POINT('Ctrl Pts',(-1.61365775139403,-0.266264900654909,
-0.311480544243686));
#4203=CARTESIAN_POINT('Ctrl Pts',(-1.62252828437015,-0.317195968905306,
-0.261368388670537));
#4204=CARTESIAN_POINT('Ctrl Pts',(-1.62691869420078,-0.33909093068465,-0.233069203882014));
#4205=CARTESIAN_POINT('Ctrl Pts',(-1.63426473152765,-0.373586846396559,
-0.174042761838764));
#4206=CARTESIAN_POINT('Ctrl Pts',(-1.63761964365402,-0.388086240756494,
-0.140365781471549));
#4207=CARTESIAN_POINT('Ctrl Pts',(-1.64212536811722,-0.407068917407805,
-0.0701778381840614));
#4208=CARTESIAN_POINT('Ctrl Pts',(-1.643248,-0.411552957311693,-0.0336652739555917));
#4209=CARTESIAN_POINT('Ctrl Pts',(-1.643248,-0.411552957311693,-2.0122792321331E-16));
#4210=CARTESIAN_POINT('Origin',(-1.675,-0.07938,-2.22044604925031E-16));
#4211=CARTESIAN_POINT('Ctrl Pts',(-1.643248,-0.411552957311693,-1.94289029309402E-16));
#4212=CARTESIAN_POINT('Ctrl Pts',(-1.643248,-0.411552957311693,0.0336652739555913));
#4213=CARTESIAN_POINT('Ctrl Pts',(-1.64212536811722,-0.407068917407805,
0.0701778381840609));
#4214=CARTESIAN_POINT('Ctrl Pts',(-1.63761964365402,-0.388086240756494,
0.140365781471549));
#4215=CARTESIAN_POINT('Ctrl Pts',(-1.63426473152765,-0.373586846396559,
0.174042761838763));
#4216=CARTESIAN_POINT('Ctrl Pts',(-1.62691869420078,-0.33909093068465,0.233069203882014));
#4217=CARTESIAN_POINT('Ctrl Pts',(-1.62252828437015,-0.317195968905306,
0.261368388670536));
#4218=CARTESIAN_POINT('Ctrl Pts',(-1.61365775139403,-0.266264900654909,
0.311480544243686));
#4219=CARTESIAN_POINT('Ctrl Pts',(-1.60919314384089,-0.237231147975235,
0.333298652394954));
#4220=CARTESIAN_POINT('Ctrl Pts',(-1.60050712143809,-0.166543350814306,
0.373030350867484));
#4221=CARTESIAN_POINT('Ctrl Pts',(-1.59665523941937,-0.123401821157026,
0.388626558458099));
#4222=CARTESIAN_POINT('Ctrl Pts',(-1.59456899932179,-0.0793800000000001,
0.397005914195118));
#4223=CARTESIAN_POINT('Origin',(0.,-0.07938,0.));
#4224=CARTESIAN_POINT('',(-1.40825612658882,-0.07938,-0.846804978391753));
#4225=CARTESIAN_POINT('Origin',(0.,-0.07938,0.));
#4226=CARTESIAN_POINT('Origin',(-1.18440385848747,-0.07938,-1.18440385848747));
#4227=CARTESIAN_POINT('Origin',(-1.18440385848747,0.,-1.18440385848747));
#4228=CARTESIAN_POINT('',(-0.846804978391753,-0.07938,-1.40825612658882));
#4229=CARTESIAN_POINT('Ctrl Pts',(-0.846804978391753,-0.0793800000000001,
-1.40825612658882));
#4230=CARTESIAN_POINT('Ctrl Pts',(-0.854205272175555,-0.123401821157026,
-1.40380622184538));
#4231=CARTESIAN_POINT('Ctrl Pts',(-0.867957148219442,-0.166543350814306,
-1.39550172959303));
#4232=CARTESIAN_POINT('Ctrl Pts',(-0.902193646979982,-0.237231147975234,
-1.3735491215176));
#4233=CARTESIAN_POINT('Ctrl Pts',(-0.920778333482564,-0.266264900654908,
-1.36127834356734));
#4234=CARTESIAN_POINT('Ctrl Pts',(-0.962485392528368,-0.317195968905306,
-1.33211611256184));
#4235=CARTESIAN_POINT('Ctrl Pts',(-0.985600426557816,-0.33909093068465,
-1.31521005565926));
#4236=CARTESIAN_POINT('Ctrl Pts',(-1.03253285680459,-0.373586846396559,
-1.27866649102984));
#4237=CARTESIAN_POINT('Ctrl Pts',(-1.05871835910697,-0.388086240756494,
-1.25722555095714));
#4238=CARTESIAN_POINT('Ctrl Pts',(-1.11153475808518,-0.407068917407805,
-1.2107812086231));
#4239=CARTESIAN_POINT('Ctrl Pts',(-1.13814686046673,-0.411552957311693,
-1.18575674747573));
#4240=CARTESIAN_POINT('Ctrl Pts',(-1.18575674747573,-0.411552957311693,
-1.13814686046673));
#4241=CARTESIAN_POINT('Ctrl Pts',(-1.2107812086231,-0.407068917407805,-1.11153475808518));
#4242=CARTESIAN_POINT('Ctrl Pts',(-1.25722555095714,-0.388086240756494,
-1.05871835910697));
#4243=CARTESIAN_POINT('Ctrl Pts',(-1.27866649102984,-0.373586846396559,
-1.03253285680459));
#4244=CARTESIAN_POINT('Ctrl Pts',(-1.31521005565926,-0.33909093068465,-0.985600426557816));
#4245=CARTESIAN_POINT('Ctrl Pts',(-1.33211611256184,-0.317195968905306,
-0.962485392528369));
#4246=CARTESIAN_POINT('Ctrl Pts',(-1.36127834356734,-0.266264900654909,
-0.920778333482565));
#4247=CARTESIAN_POINT('Ctrl Pts',(-1.3735491215176,-0.237231147975234,-0.902193646979983));
#4248=CARTESIAN_POINT('Ctrl Pts',(-1.39550172959303,-0.166543350814306,
-0.867957148219442));
#4249=CARTESIAN_POINT('Ctrl Pts',(-1.40380622184538,-0.123401821157026,
-0.854205272175555));
#4250=CARTESIAN_POINT('Ctrl Pts',(-1.40825612658882,-0.07938,-0.846804978391753));
#4251=CARTESIAN_POINT('Origin',(-1.18440385848747,-0.07938,-1.18440385848747));
#4252=CARTESIAN_POINT('Origin',(0.,-0.07938,0.));
#4253=CARTESIAN_POINT('',(-0.397005914195118,-0.07938,-1.59456899932179));
#4254=CARTESIAN_POINT('Origin',(0.,-0.07938,0.));
#4255=CARTESIAN_POINT('Origin',(1.11022302462516E-16,-0.07938,-1.675));
#4256=CARTESIAN_POINT('Origin',(1.11022302462516E-16,0.,-1.675));
#4257=CARTESIAN_POINT('',(0.397005914195118,-0.07938,-1.59456899932179));
#4258=CARTESIAN_POINT('Ctrl Pts',(0.397005914195119,-0.0793800000000001,
-1.59456899932179));
#4259=CARTESIAN_POINT('Ctrl Pts',(0.388626558458099,-0.123401821157026,
-1.59665523941937));
#4260=CARTESIAN_POINT('Ctrl Pts',(0.373030350867485,-0.166543350814306,
-1.60050712143809));
#4261=CARTESIAN_POINT('Ctrl Pts',(0.333298652394954,-0.237231147975234,
-1.60919314384089));
#4262=CARTESIAN_POINT('Ctrl Pts',(0.311480544243686,-0.266264900654909,
-1.61365775139403));
#4263=CARTESIAN_POINT('Ctrl Pts',(0.261368388670537,-0.317195968905306,
-1.62252828437015));
#4264=CARTESIAN_POINT('Ctrl Pts',(0.233069203882014,-0.33909093068465,-1.62691869420078));
#4265=CARTESIAN_POINT('Ctrl Pts',(0.174042761838763,-0.373586846396559,
-1.63426473152765));
#4266=CARTESIAN_POINT('Ctrl Pts',(0.140365781471549,-0.388086240756494,
-1.63761964365402));
#4267=CARTESIAN_POINT('Ctrl Pts',(0.0701778381840612,-0.407068917407805,
-1.64212536811722));
#4268=CARTESIAN_POINT('Ctrl Pts',(0.0336652739555916,-0.411552957311693,
-1.643248));
#4269=CARTESIAN_POINT('Ctrl Pts',(-0.0336652739555915,-0.411552957311693,
-1.643248));
#4270=CARTESIAN_POINT('Ctrl Pts',(-0.0701778381840612,-0.407068917407805,
-1.64212536811722));
#4271=CARTESIAN_POINT('Ctrl Pts',(-0.140365781471549,-0.388086240756494,
-1.63761964365402));
#4272=CARTESIAN_POINT('Ctrl Pts',(-0.174042761838764,-0.373586846396559,
-1.63426473152765));
#4273=CARTESIAN_POINT('Ctrl Pts',(-0.233069203882014,-0.33909093068465,
-1.62691869420078));
#4274=CARTESIAN_POINT('Ctrl Pts',(-0.261368388670536,-0.317195968905306,
-1.62252828437015));
#4275=CARTESIAN_POINT('Ctrl Pts',(-0.311480544243686,-0.266264900654908,
-1.61365775139403));
#4276=CARTESIAN_POINT('Ctrl Pts',(-0.333298652394954,-0.237231147975234,
-1.60919314384089));
#4277=CARTESIAN_POINT('Ctrl Pts',(-0.373030350867485,-0.166543350814306,
-1.60050712143809));
#4278=CARTESIAN_POINT('Ctrl Pts',(-0.388626558458099,-0.123401821157026,
-1.59665523941937));
#4279=CARTESIAN_POINT('Ctrl Pts',(-0.397005914195118,-0.07938,-1.59456899932179));
#4280=CARTESIAN_POINT('Origin',(1.11022302462516E-16,-0.07938,-1.675));
#4281=CARTESIAN_POINT('Origin',(0.,-0.07938,0.));
#4282=CARTESIAN_POINT('',(0.846804978391753,-0.07938,-1.40825612658882));
#4283=CARTESIAN_POINT('Origin',(0.,-0.07938,0.));
#4284=CARTESIAN_POINT('Origin',(1.18440385848747,-0.07938,-1.18440385848747));
#4285=CARTESIAN_POINT('Origin',(1.18440385848747,0.,-1.18440385848747));
#4286=CARTESIAN_POINT('',(1.40825612658882,-0.07938,-0.846804978391753));
#4287=CARTESIAN_POINT('Ctrl Pts',(1.40825612658882,-0.0793800000000001,
-0.846804978391753));
#4288=CARTESIAN_POINT('Ctrl Pts',(1.40380622184538,-0.123401821157026,-0.854205272175555));
#4289=CARTESIAN_POINT('Ctrl Pts',(1.39550172959303,-0.166543350814306,-0.867957148219442));
#4290=CARTESIAN_POINT('Ctrl Pts',(1.3735491215176,-0.237231147975234,-0.902193646979983));
#4291=CARTESIAN_POINT('Ctrl Pts',(1.36127834356734,-0.266264900654908,-0.920778333482565));
#4292=CARTESIAN_POINT('Ctrl Pts',(1.33211611256184,-0.317195968905306,-0.962485392528369));
#4293=CARTESIAN_POINT('Ctrl Pts',(1.31521005565926,-0.33909093068465,-0.985600426557816));
#4294=CARTESIAN_POINT('Ctrl Pts',(1.27866649102984,-0.373586846396559,-1.03253285680459));
#4295=CARTESIAN_POINT('Ctrl Pts',(1.25722555095714,-0.388086240756494,-1.05871835910697));
#4296=CARTESIAN_POINT('Ctrl Pts',(1.2107812086231,-0.407068917407805,-1.11153475808518));
#4297=CARTESIAN_POINT('Ctrl Pts',(1.18575674747573,-0.411552957311693,-1.13814686046673));
#4298=CARTESIAN_POINT('Ctrl Pts',(1.13814686046673,-0.411552957311693,-1.18575674747573));
#4299=CARTESIAN_POINT('Ctrl Pts',(1.11153475808518,-0.407068917407805,-1.2107812086231));
#4300=CARTESIAN_POINT('Ctrl Pts',(1.05871835910697,-0.388086240756494,-1.25722555095714));
#4301=CARTESIAN_POINT('Ctrl Pts',(1.03253285680459,-0.373586846396559,-1.27866649102984));
#4302=CARTESIAN_POINT('Ctrl Pts',(0.985600426557816,-0.33909093068465,-1.31521005565926));
#4303=CARTESIAN_POINT('Ctrl Pts',(0.962485392528369,-0.317195968905306,
-1.33211611256184));
#4304=CARTESIAN_POINT('Ctrl Pts',(0.920778333482565,-0.266264900654909,
-1.36127834356734));
#4305=CARTESIAN_POINT('Ctrl Pts',(0.902193646979983,-0.237231147975234,
-1.3735491215176));
#4306=CARTESIAN_POINT('Ctrl Pts',(0.867957148219442,-0.166543350814306,
-1.39550172959303));
#4307=CARTESIAN_POINT('Ctrl Pts',(0.854205272175555,-0.123401821157026,
-1.40380622184538));
#4308=CARTESIAN_POINT('Ctrl Pts',(0.846804978391753,-0.0793800000000001,
-1.40825612658882));
#4309=CARTESIAN_POINT('Origin',(1.18440385848747,-0.07938,-1.18440385848747));
#4310=CARTESIAN_POINT('Origin',(0.,-0.27783,0.));
#4311=CARTESIAN_POINT('',(-1.643248,-0.47628,2.01239840340529E-16));
#4312=CARTESIAN_POINT('Origin',(0.,-0.47628,0.));
#4313=CARTESIAN_POINT('',(-1.643248,-0.27783,2.01239840340529E-16));
#4314=CARTESIAN_POINT('',(1.59456899932179,-0.07938,0.397005914195118));
#4315=CARTESIAN_POINT('Origin',(0.,-0.07938,0.));
#4316=CARTESIAN_POINT('',(1.59456899932179,-0.07938,-0.397005914195118));
#4317=CARTESIAN_POINT('Ctrl Pts',(1.59456899932179,-0.0793800000000001,
0.397005914195118));
#4318=CARTESIAN_POINT('Ctrl Pts',(1.59665523941937,-0.123401821157026,0.388626558458099));
#4319=CARTESIAN_POINT('Ctrl Pts',(1.60050712143809,-0.166543350814306,0.373030350867485));
#4320=CARTESIAN_POINT('Ctrl Pts',(1.60919314384089,-0.237231147975234,0.333298652394954));
#4321=CARTESIAN_POINT('Ctrl Pts',(1.61365775139403,-0.266264900654909,0.311480544243686));
#4322=CARTESIAN_POINT('Ctrl Pts',(1.62252828437015,-0.317195968905306,0.261368388670537));
#4323=CARTESIAN_POINT('Ctrl Pts',(1.62691869420078,-0.33909093068465,0.233069203882014));
#4324=CARTESIAN_POINT('Ctrl Pts',(1.63426473152765,-0.373586846396559,0.174042761838764));
#4325=CARTESIAN_POINT('Ctrl Pts',(1.63761964365402,-0.388086240756494,0.140365781471549));
#4326=CARTESIAN_POINT('Ctrl Pts',(1.64212536811722,-0.407068917407805,0.0701778381840612));
#4327=CARTESIAN_POINT('Ctrl Pts',(1.643248,-0.411552957311693,0.0336652739555916));
#4328=CARTESIAN_POINT('Ctrl Pts',(1.643248,-0.411552957311693,-0.0336652739555916));
#4329=CARTESIAN_POINT('Ctrl Pts',(1.64212536811722,-0.407068917407805,-0.0701778381840612));
#4330=CARTESIAN_POINT('Ctrl Pts',(1.63761964365402,-0.388086240756494,-0.140365781471549));
#4331=CARTESIAN_POINT('Ctrl Pts',(1.63426473152765,-0.373586846396559,-0.174042761838764));
#4332=CARTESIAN_POINT('Ctrl Pts',(1.62691869420078,-0.33909093068465,-0.233069203882014));
#4333=CARTESIAN_POINT('Ctrl Pts',(1.62252828437015,-0.317195968905306,-0.261368388670537));
#4334=CARTESIAN_POINT('Ctrl Pts',(1.61365775139403,-0.266264900654909,-0.311480544243686));
#4335=CARTESIAN_POINT('Ctrl Pts',(1.60919314384089,-0.237231147975234,-0.333298652394954));
#4336=CARTESIAN_POINT('Ctrl Pts',(1.60050712143809,-0.166543350814306,-0.373030350867485));
#4337=CARTESIAN_POINT('Ctrl Pts',(1.59665523941937,-0.123401821157026,-0.388626558458099));
#4338=CARTESIAN_POINT('Ctrl Pts',(1.59456899932179,-0.07938,-0.397005914195118));
#4339=CARTESIAN_POINT('Origin',(0.,-0.07938,0.));
#4340=CARTESIAN_POINT('Origin',(0.,-0.07938,0.));
#4341=CARTESIAN_POINT('Origin',(1.675,-0.07938,0.));
#4342=CARTESIAN_POINT('Origin',(1.675,0.,0.));
#4343=CARTESIAN_POINT('Origin',(1.675,-0.07938,0.));
#4344=CARTESIAN_POINT('Origin',(0.,-0.47628,0.));
#4345=CARTESIAN_POINT('Origin',(0.,-0.07938,0.));
#4346=CARTESIAN_POINT('',(0.,0.,0.));
#4347=CARTESIAN_POINT('Origin',(1.70469,0.695,0.));
#4348=CARTESIAN_POINT('',(-1.70469,0.695,-2.0876431520385E-16));
#4349=CARTESIAN_POINT('Origin',(0.,0.695,0.));
#4350=CARTESIAN_POINT('',(-1.65031,0.695,-2.02104685910087E-16));
#4351=CARTESIAN_POINT('Origin',(0.,0.695,0.));
#4352=CARTESIAN_POINT('Origin',(0.,0.6575,0.));
#4353=CARTESIAN_POINT('',(-1.70469,0.62,-2.0876431520385E-16));
#4354=CARTESIAN_POINT('Origin',(0.,0.62,0.));
#4355=CARTESIAN_POINT('',(-1.70469,0.6575,-2.0876431520385E-16));
#4356=CARTESIAN_POINT('Origin',(1.65031,0.62,0.));
#4357=CARTESIAN_POINT('',(-1.65031,0.62,-2.02104685910087E-16));
#4358=CARTESIAN_POINT('Origin',(0.,0.62,0.));
#4359=CARTESIAN_POINT('Origin',(0.,0.6575,0.));
#4360=CARTESIAN_POINT('',(-1.65031,0.6575,-2.02104685910087E-16));
#4361=CARTESIAN_POINT('Origin',(1.70469,-0.62,0.));
#4362=CARTESIAN_POINT('',(-1.70469,-0.62,-2.0876431520385E-16));
#4363=CARTESIAN_POINT('Origin',(0.,-0.62,0.));
#4364=CARTESIAN_POINT('',(-1.65031,-0.62,-2.02104685910087E-16));
#4365=CARTESIAN_POINT('Origin',(0.,-0.62,0.));
#4366=CARTESIAN_POINT('Origin',(0.,-0.6575,0.));
#4367=CARTESIAN_POINT('',(-1.70469,-0.695,-2.0876431520385E-16));
#4368=CARTESIAN_POINT('Origin',(0.,-0.695,0.));
#4369=CARTESIAN_POINT('',(-1.70469,-0.6575,-2.0876431520385E-16));
#4370=CARTESIAN_POINT('Origin',(1.65031,-0.695,0.));
#4371=CARTESIAN_POINT('',(-1.65031,-0.695,-2.02104685910087E-16));
#4372=CARTESIAN_POINT('Origin',(0.,-0.695,0.));
#4373=CARTESIAN_POINT('Origin',(0.,-0.6575,0.));
#4374=CARTESIAN_POINT('',(-1.65031,-0.6575,-2.02104685910087E-16));
#4375=CARTESIAN_POINT('',(0.,0.,0.));
#4376=CARTESIAN_POINT('',(0.,0.,0.));
#4377=CARTESIAN_POINT('',(0.,0.,0.));
#4378=CARTESIAN_POINT('',(0.,0.,0.));
#4379=CARTESIAN_POINT('',(0.,0.,0.));
#4380=CARTESIAN_POINT('',(0.,0.,0.));
#4381=CARTESIAN_POINT('Origin',(0.,1.7,4.5));
#4382=CARTESIAN_POINT('',(-1.75,4.3,4.5));
#4383=CARTESIAN_POINT('Origin',(0.,4.3,4.5));
#4384=CARTESIAN_POINT('',(-1.75,1.7,4.5));
#4385=CARTESIAN_POINT('',(-1.75,1.7,4.5));
#4386=CARTESIAN_POINT('Origin',(0.,1.7,4.5));
#4387=CARTESIAN_POINT('Origin',(0.,1.7,4.5));
#4388=CARTESIAN_POINT('',(-2.34,4.3,4.5));
#4389=CARTESIAN_POINT('Origin',(0.,4.3,4.5));
#4390=CARTESIAN_POINT('',(-2.34,1.7,4.5));
#4391=CARTESIAN_POINT('',(-2.34,1.7,4.5));
#4392=CARTESIAN_POINT('Origin',(0.,1.7,4.5));
#4393=CARTESIAN_POINT('Origin',(0.,4.3,4.5));
#4394=CARTESIAN_POINT('Origin',(0.,1.7,4.5));
#4395=CARTESIAN_POINT('',(0.,0.,0.));
#4396=CARTESIAN_POINT('Origin',(-2.8,-0.5,4.5));
#4397=CARTESIAN_POINT('',(-3.025,-0.4,4.5));
#4398=CARTESIAN_POINT('Origin',(-2.8,-0.4,4.5));
#4399=CARTESIAN_POINT('',(-3.025,0.,4.5));
#4400=CARTESIAN_POINT('',(-3.025,-0.5,4.5));
#4401=CARTESIAN_POINT('Origin',(-2.8,0.,4.5));
#4402=CARTESIAN_POINT('Origin',(1.71450551880629E-16,-0.5,7.3));
#4403=CARTESIAN_POINT('',(-0.225,-0.4,7.3));
#4404=CARTESIAN_POINT('Origin',(1.71450551880629E-16,-0.4,7.3));
#4405=CARTESIAN_POINT('',(-0.225,0.,7.3));
#4406=CARTESIAN_POINT('',(-0.225,-0.5,7.3));
#4407=CARTESIAN_POINT('Origin',(1.71450551880629E-16,0.,7.3));
#4408=CARTESIAN_POINT('Origin',(2.8,-0.5,4.5));
#4409=CARTESIAN_POINT('',(2.575,-0.4,4.5));
#4410=CARTESIAN_POINT('Origin',(2.8,-0.4,4.5));
#4411=CARTESIAN_POINT('',(2.575,0.,4.5));
#4412=CARTESIAN_POINT('',(2.575,-0.5,4.5));
#4413=CARTESIAN_POINT('Origin',(2.8,0.,4.5));
#4414=CARTESIAN_POINT('Origin',(-5.14351655641888E-16,-0.5,1.7));
#4415=CARTESIAN_POINT('',(-0.225000000000001,-0.4,1.7));
#4416=CARTESIAN_POINT('Origin',(-5.14351655641888E-16,-0.4,1.7));
#4417=CARTESIAN_POINT('',(-0.225000000000001,0.,1.7));
#4418=CARTESIAN_POINT('',(-0.225000000000001,-0.5,1.7));
#4419=CARTESIAN_POINT('Origin',(-5.14351655641888E-16,0.,1.7));
#4420=CARTESIAN_POINT('Origin',(0.,0.,4.5));
#4421=CARTESIAN_POINT('',(-2.34,0.3,4.5));
#4422=CARTESIAN_POINT('Origin',(0.,0.3,4.5));
#4423=CARTESIAN_POINT('',(-2.34,0.,4.5));
#4424=CARTESIAN_POINT('',(-2.34,0.,4.5));
#4425=CARTESIAN_POINT('Origin',(0.,0.,4.5));
#4426=CARTESIAN_POINT('Origin',(0.,0.3,4.5));
#4427=CARTESIAN_POINT('',(-1.6,0.3,4.5));
#4428=CARTESIAN_POINT('Origin',(0.,0.3,4.5));
#4429=CARTESIAN_POINT('Origin',(0.,-0.41,4.5));
#4430=CARTESIAN_POINT('',(-1.8,-0.4,4.5));
#4431=CARTESIAN_POINT('Origin',(0.,-0.4,4.5));
#4432=CARTESIAN_POINT('',(-1.8,-0.2,4.5));
#4433=CARTESIAN_POINT('',(-1.8,-0.41,4.5));
#4434=CARTESIAN_POINT('Origin',(0.,-0.2,4.5));
#4435=CARTESIAN_POINT('Origin',(0.,-0.2,4.5));
#4436=CARTESIAN_POINT('',(-1.6,-0.2,4.5));
#4437=CARTESIAN_POINT('Origin',(0.,-0.2,4.5));
#4438=CARTESIAN_POINT('Origin',(0.,-0.4,4.5));
#4439=CARTESIAN_POINT('',(-1.6,-0.4,4.5));
#4440=CARTESIAN_POINT('Origin',(0.,-0.4,4.5));
#4441=CARTESIAN_POINT('',(-3.5,0.,4.5));
#4442=CARTESIAN_POINT('Origin',(0.,0.,4.5));
#4443=CARTESIAN_POINT('',(-3.5,-0.4,4.5));
#4444=CARTESIAN_POINT('',(-3.5,-0.4,4.5));
#4445=CARTESIAN_POINT('Origin',(0.,-0.4,4.5));
#4446=CARTESIAN_POINT('Origin',(0.,0.,4.5));
#4447=CARTESIAN_POINT('Origin',(0.,-0.4,4.5));
#4448=CARTESIAN_POINT('',(0.,0.,0.));
#4449=CARTESIAN_POINT('Origin',(0.,-0.4,4.5));
#4450=CARTESIAN_POINT('',(-1.,-0.2,4.5));
#4451=CARTESIAN_POINT('Origin',(0.,-0.2,4.5));
#4452=CARTESIAN_POINT('',(-1.,-0.4,4.5));
#4453=CARTESIAN_POINT('',(-1.,-0.4,4.5));
#4454=CARTESIAN_POINT('Origin',(0.,-0.4,4.5));
#4455=CARTESIAN_POINT('Origin',(0.,-0.4,4.5));
#4456=CARTESIAN_POINT('',(-1.8,-0.2,4.5));
#4457=CARTESIAN_POINT('Origin',(0.,-0.2,4.5));
#4458=CARTESIAN_POINT('',(-1.8,-0.4,4.5));
#4459=CARTESIAN_POINT('',(-1.8,-0.4,4.5));
#4460=CARTESIAN_POINT('Origin',(0.,-0.4,4.5));
#4461=CARTESIAN_POINT('Origin',(0.,-0.2,4.5));
#4462=CARTESIAN_POINT('Origin',(0.,-0.4,4.5));
#4463=CARTESIAN_POINT('',(0.,0.,0.));
#4464=CARTESIAN_POINT('Origin',(-2.8,5.9,4.5));
#4465=CARTESIAN_POINT('',(-3.025,6.,4.5));
#4466=CARTESIAN_POINT('Origin',(-2.8,6.,4.5));
#4467=CARTESIAN_POINT('',(-3.025,6.4,4.5));
#4468=CARTESIAN_POINT('',(-3.025,5.9,4.5));
#4469=CARTESIAN_POINT('Origin',(-2.8,6.4,4.5));
#4470=CARTESIAN_POINT('Origin',(1.71450551880629E-16,5.9,7.3));
#4471=CARTESIAN_POINT('',(-0.225,6.,7.3));
#4472=CARTESIAN_POINT('Origin',(1.71450551880629E-16,6.,7.3));
#4473=CARTESIAN_POINT('',(-0.225,6.4,7.3));
#4474=CARTESIAN_POINT('',(-0.225,5.9,7.3));
#4475=CARTESIAN_POINT('Origin',(1.71450551880629E-16,6.4,7.3));
#4476=CARTESIAN_POINT('Origin',(2.8,5.9,4.5));
#4477=CARTESIAN_POINT('',(2.575,6.,4.5));
#4478=CARTESIAN_POINT('Origin',(2.8,6.,4.5));
#4479=CARTESIAN_POINT('',(2.575,6.4,4.5));
#4480=CARTESIAN_POINT('',(2.575,5.9,4.5));
#4481=CARTESIAN_POINT('Origin',(2.8,6.4,4.5));
#4482=CARTESIAN_POINT('Origin',(-5.14351655641888E-16,5.9,1.7));
#4483=CARTESIAN_POINT('',(-0.225000000000001,6.,1.7));
#4484=CARTESIAN_POINT('Origin',(-5.14351655641888E-16,6.,1.7));
#4485=CARTESIAN_POINT('',(-0.225000000000001,6.4,1.7));
#4486=CARTESIAN_POINT('',(-0.225000000000001,5.9,1.7));
#4487=CARTESIAN_POINT('Origin',(-5.14351655641888E-16,6.4,1.7));
#4488=CARTESIAN_POINT('Origin',(0.,5.7,4.5));
#4489=CARTESIAN_POINT('',(-2.34,6.,4.5));
#4490=CARTESIAN_POINT('Origin',(0.,6.,4.5));
#4491=CARTESIAN_POINT('',(-2.34,5.7,4.5));
#4492=CARTESIAN_POINT('',(-2.34,5.7,4.5));
#4493=CARTESIAN_POINT('Origin',(0.,5.7,4.5));
#4494=CARTESIAN_POINT('Origin',(0.,5.7,4.5));
#4495=CARTESIAN_POINT('',(-1.8,5.7,4.5));
#4496=CARTESIAN_POINT('Origin',(0.,5.7,4.5));
#4497=CARTESIAN_POINT('Origin',(0.,6.,4.5));
#4498=CARTESIAN_POINT('',(-1.8,6.4,4.5));
#4499=CARTESIAN_POINT('Origin',(0.,6.4,4.5));
#4500=CARTESIAN_POINT('',(-1.8,6.,4.5));
#4501=CARTESIAN_POINT('Origin',(0.,6.,4.5));
#4502=CARTESIAN_POINT('',(-3.5,6.4,4.5));
#4503=CARTESIAN_POINT('Origin',(0.,6.4,4.5));
#4504=CARTESIAN_POINT('',(-3.5,6.,4.5));
#4505=CARTESIAN_POINT('',(-3.5,6.,4.5));
#4506=CARTESIAN_POINT('Origin',(0.,6.,4.5));
#4507=CARTESIAN_POINT('Origin',(0.,6.4,4.5));
#4508=CARTESIAN_POINT('Origin',(0.,6.,4.5));
#4509=CARTESIAN_POINT('',(0.,0.,0.));
#4510=CARTESIAN_POINT('Origin',(0.3,0.4,0.));
#4511=CARTESIAN_POINT('',(-0.3,0.4,-3.67394039744206E-17));
#4512=CARTESIAN_POINT('Origin',(0.,0.4,0.));
#4513=CARTESIAN_POINT('Origin',(0.,0.375,0.));
#4514=CARTESIAN_POINT('',(-0.35,0.35,-4.28626379701573E-17));
#4515=CARTESIAN_POINT('Origin',(0.,0.35,0.));
#4516=CARTESIAN_POINT('',(-0.325,0.375,-3.9801020972289E-17));
#4517=CARTESIAN_POINT('Origin',(0.,0.19,0.));
#4518=CARTESIAN_POINT('',(-0.35,0.03,-4.28626379701574E-17));
#4519=CARTESIAN_POINT('Origin',(0.,0.03,0.));
#4520=CARTESIAN_POINT('',(-0.35,0.19,-4.28626379701574E-17));
#4521=CARTESIAN_POINT('Origin',(0.,0.0149999999999999,0.));
#4522=CARTESIAN_POINT('',(-0.32,-3.29597460435593E-17,-3.91886975727153E-17));
#4523=CARTESIAN_POINT('Origin',(0.,0.,0.));
#4524=CARTESIAN_POINT('',(-0.335,0.0149999999999999,-4.10256677714363E-17));
#4525=CARTESIAN_POINT('Origin',(0.22,0.,0.));
#4526=CARTESIAN_POINT('',(-0.22,-6.93889390390723E-18,-2.69422295812418E-17));
#4527=CARTESIAN_POINT('Origin',(0.,0.,0.));
#4528=CARTESIAN_POINT('Origin',(0.,-0.02,0.));
#4529=CARTESIAN_POINT('',(-0.1954,-0.0492,2.39295984553393E-17));
#4530=CARTESIAN_POINT('Origin',(0.,-0.0492,0.));
#4531=CARTESIAN_POINT('',(-0.21,-0.02,-2.57175827820944E-17));
#4532=CARTESIAN_POINT('Origin',(0.,-0.8,0.));
#4533=CARTESIAN_POINT('',(-0.1954,-1.5646,2.39295984553393E-17));
#4534=CARTESIAN_POINT('Origin',(0.,-1.5646,0.));
#4535=CARTESIAN_POINT('',(-0.1954,-0.8,-2.39295984553393E-17));
#4536=CARTESIAN_POINT('Origin',(0.,-1.58,0.));
#4537=CARTESIAN_POINT('',(-0.16,-1.6,-1.95943487863577E-17));
#4538=CARTESIAN_POINT('Origin',(0.,-1.6,0.));
#4539=CARTESIAN_POINT('',(-0.18,-1.58,-2.20436423846524E-17));
#4540=CARTESIAN_POINT('Origin',(0.,-1.6,0.));
#4541=CARTESIAN_POINT('Origin',(0.0866025403784439,-0.4,-0.15));
#4542=CARTESIAN_POINT('',(0.173205080756888,-0.4,0.));
#4543=CARTESIAN_POINT('',(0.0866025403784439,-0.4,-0.15));
#4544=CARTESIAN_POINT('',(0.173205080756888,-0.4,0.));
#4545=CARTESIAN_POINT('',(0.0866025403784439,-0.64,-0.15));
#4546=CARTESIAN_POINT('',(0.0866025403784439,-0.4,-0.15));
#4547=CARTESIAN_POINT('',(0.173205080756888,-0.64,0.));
#4548=CARTESIAN_POINT('',(0.173205080756888,-0.64,0.));
#4549=CARTESIAN_POINT('',(0.173205080756888,-0.4,0.));
#4550=CARTESIAN_POINT('Origin',(-0.0866025403784438,-0.4,-0.15));
#4551=CARTESIAN_POINT('',(-0.0866025403784438,-0.4,-0.15));
#4552=CARTESIAN_POINT('',(0.0866025403784439,-0.4,-0.15));
#4553=CARTESIAN_POINT('',(-0.0866025403784438,-0.64,-0.15));
#4554=CARTESIAN_POINT('',(-0.0866025403784438,-0.4,-0.15));
#4555=CARTESIAN_POINT('',(0.0866025403784439,-0.64,-0.15));
#4556=CARTESIAN_POINT('Origin',(-0.173205080756888,-0.4,-2.77555756156289E-17));
#4557=CARTESIAN_POINT('',(-0.173205080756888,-0.4,-2.12115047744981E-17));
#4558=CARTESIAN_POINT('',(-0.0866025403784438,-0.4,-0.15));
#4559=CARTESIAN_POINT('',(-0.173205080756888,-0.64,-2.77555756156289E-17));
#4560=CARTESIAN_POINT('',(-0.173205080756888,-0.4,-2.12115047744981E-17));
#4561=CARTESIAN_POINT('',(-0.0866025403784438,-0.64,-0.15));
#4562=CARTESIAN_POINT('Origin',(-0.0866025403784439,-0.4,0.15));
#4563=CARTESIAN_POINT('',(-0.0866025403784439,-0.4,0.15));
#4564=CARTESIAN_POINT('',(-0.173205080756888,-0.4,-2.12115047744981E-17));
#4565=CARTESIAN_POINT('',(-0.0866025403784439,-0.64,0.15));
#4566=CARTESIAN_POINT('',(-0.0866025403784439,-0.4,0.15));
#4567=CARTESIAN_POINT('',(-0.173205080756888,-0.64,-2.12115047744981E-17));
#4568=CARTESIAN_POINT('Origin',(0.0866025403784439,-0.4,0.15));
#4569=CARTESIAN_POINT('',(0.0866025403784439,-0.4,0.15));
#4570=CARTESIAN_POINT('',(-0.0866025403784439,-0.4,0.15));
#4571=CARTESIAN_POINT('',(0.0866025403784439,-0.64,0.15));
#4572=CARTESIAN_POINT('',(0.0866025403784439,-0.4,0.15));
#4573=CARTESIAN_POINT('',(-0.0866025403784439,-0.64,0.15));
#4574=CARTESIAN_POINT('Origin',(0.173205080756888,-0.4,0.));
#4575=CARTESIAN_POINT('',(0.0866025403784439,-0.4,0.15));
#4576=CARTESIAN_POINT('',(0.0866025403784439,-0.64,0.15));
#4577=CARTESIAN_POINT('Origin',(0.,-0.4,-2.77555756156289E-17));
#4578=CARTESIAN_POINT('Origin',(0.,-0.64,-2.77555756156289E-17));
#4579=CARTESIAN_POINT('',(0.,0.,0.));
#4580=CARTESIAN_POINT('',(0.,1.,4.5));
#4581=CARTESIAN_POINT('',(0.,5.,4.5));
#4582=CARTESIAN_POINT('',(0.,0.,0.));
#4583=CARTESIAN_POINT('',(0.,0.,0.));
#4584=CARTESIAN_POINT('',(0.,0.,0.));
#4585=CARTESIAN_POINT('',(0.,0.,0.));
#4586=CARTESIAN_POINT('',(2.8,-0.4,4.5));
#4587=CARTESIAN_POINT('',(2.8,6.4,4.5));
#4588=CARTESIAN_POINT('',(0.,-0.4,7.3));
#4589=CARTESIAN_POINT('',(4.44089209850063E-16,6.4,7.3));
#4590=CARTESIAN_POINT('',(-2.8,-0.4,4.5));
#4591=CARTESIAN_POINT('',(-2.8,6.4,4.5));
#4592=CARTESIAN_POINT('',(-4.44089209850063E-16,-0.4,1.7));
#4593=CARTESIAN_POINT('',(-4.44089209850063E-16,6.4,1.7));
#4594=CARTESIAN_POINT('',(0.,0.,0.));
#4595=CARTESIAN_POINT('',(0.,0.,0.));
#4596=CARTESIAN_POINT('Origin',(0.,6.4,4.5));
#4597=CARTESIAN_POINT('',(-0.95,6.4,4.5));
#4598=CARTESIAN_POINT('Origin',(0.,6.4,4.5));
#4599=CARTESIAN_POINT('',(-0.95,6.52,4.5));
#4600=CARTESIAN_POINT('',(-0.95,6.4,4.5));
#4601=CARTESIAN_POINT('Origin',(0.,6.52,4.5));
#4602=CARTESIAN_POINT('Origin',(0.,6.52,4.5));
#4603=CARTESIAN_POINT('',(-1.,6.52,4.5));
#4604=CARTESIAN_POINT('Origin',(0.,6.52,4.5));
#4605=CARTESIAN_POINT('Origin',(0.,6.4,4.5));
#4606=CARTESIAN_POINT('',(-1.,6.4,4.5));
#4607=CARTESIAN_POINT('Origin',(0.,6.4,4.5));
#4608=CARTESIAN_POINT('Origin',(0.,-2.5,4.5));
#4609=CARTESIAN_POINT('',(-1.,0.3,4.5));
#4610=CARTESIAN_POINT('',(-1.,-2.5,4.5));
#4611=CARTESIAN_POINT('Origin',(0.,0.3,4.5));
#4612=CARTESIAN_POINT('Origin',(0.,0.3,4.5));
#4613=CARTESIAN_POINT('',(-1.2,0.3,4.5));
#4614=CARTESIAN_POINT('Origin',(0.,0.3,4.5));
#4615=CARTESIAN_POINT('Origin',(0.,0.,4.5));
#4616=CARTESIAN_POINT('',(-1.2,0.,4.5));
#4617=CARTESIAN_POINT('Origin',(0.,0.,4.5));
#4618=CARTESIAN_POINT('',(-1.,0.,4.5));
#4619=CARTESIAN_POINT('Origin',(0.,0.,4.5));
#4620=CARTESIAN_POINT('Origin',(0.,0.,4.5));
#4621=CARTESIAN_POINT('',(-1.2,0.,4.5));
#4622=CARTESIAN_POINT('Origin',(0.,-2.5,4.5));
#4623=CARTESIAN_POINT('',(-1.,-2.5,4.5));
#4624=CARTESIAN_POINT('',(-1.,-2.5,4.5));
#4625=CARTESIAN_POINT('Origin',(0.,-2.5,4.5));
#4626=CARTESIAN_POINT('Origin',(0.,-2.5,4.5));
#4627=CARTESIAN_POINT('',(-1.,7.5,4.5));
#4628=CARTESIAN_POINT('Origin',(0.,7.5,4.5));
#4629=CARTESIAN_POINT('',(-1.,-2.5,4.5));
#4630=CARTESIAN_POINT('Origin',(0.,7.5,4.5));
#4631=CARTESIAN_POINT('Origin',(0.,-2.5,4.5));
#4632=CARTESIAN_POINT('',(0.,0.,0.));
#4633=CARTESIAN_POINT('Origin',(0.,5.7,4.5));
#4634=CARTESIAN_POINT('',(-1.01,6.4,4.5));
#4635=CARTESIAN_POINT('Origin',(0.,6.4,4.5));
#4636=CARTESIAN_POINT('',(-1.01,5.7,4.5));
#4637=CARTESIAN_POINT('',(-1.01,5.7,4.5));
#4638=CARTESIAN_POINT('Origin',(0.,5.7,4.5));
#4639=CARTESIAN_POINT('Origin',(0.,5.7,4.5));
#4640=CARTESIAN_POINT('',(-1.35,6.4,4.5));
#4641=CARTESIAN_POINT('Origin',(0.,6.4,4.5));
#4642=CARTESIAN_POINT('',(-1.35,5.7,4.5));
#4643=CARTESIAN_POINT('',(-1.35,5.7,4.5));
#4644=CARTESIAN_POINT('Origin',(0.,5.7,4.5));
#4645=CARTESIAN_POINT('Origin',(0.,6.4,4.5));
#4646=CARTESIAN_POINT('Origin',(0.,5.7,4.5));
#4647=CARTESIAN_POINT('',(0.,0.,0.));
#4648=CARTESIAN_POINT('Origin',(0.,0.,-0.1));
#4649=CARTESIAN_POINT('',(-0.885408350996075,0.344313885846057,0.));
#4650=CARTESIAN_POINT('',(-0.885408350996075,0.344313885846057,0.12));
#4651=CARTESIAN_POINT('',(-0.885408350996075,0.344313885846057,-0.1));
#4652=CARTESIAN_POINT('',(-0.885408350996075,-0.344313885846057,0.));
#4653=CARTESIAN_POINT('Origin',(0.,0.,0.));
#4654=CARTESIAN_POINT('',(-0.885408350996075,-0.344313885846057,0.12));
#4655=CARTESIAN_POINT('',(-0.885408350996075,-0.344313885846057,-0.1));
#4656=CARTESIAN_POINT('Origin',(0.,0.,0.12));
#4657=CARTESIAN_POINT('Origin',(-0.947327569834341,-0.493147518935016,0.));
#4658=CARTESIAN_POINT('',(-0.8680312528477,-0.633495422775274,0.));
#4659=CARTESIAN_POINT('Origin',(-0.947327569834341,-0.493147518935016,0.));
#4660=CARTESIAN_POINT('',(-0.8680312528477,-0.633495422775274,0.12));
#4661=CARTESIAN_POINT('Ctrl Pts',(-0.8680312528477,-0.633495422775274,0.12));
#4662=CARTESIAN_POINT('Ctrl Pts',(-0.8680312528477,-0.633495422775274,0.1));
#4663=CARTESIAN_POINT('Ctrl Pts',(-0.8680312528477,-0.633495422775274,0.08));
#4664=CARTESIAN_POINT('Ctrl Pts',(-0.8680312528477,-0.633495422775274,0.04));
#4665=CARTESIAN_POINT('Ctrl Pts',(-0.8680312528477,-0.633495422775274,0.02));
#4666=CARTESIAN_POINT('Ctrl Pts',(-0.8680312528477,-0.633495422775274,0.));
#4667=CARTESIAN_POINT('Origin',(-0.947327569834341,-0.493147518935016,0.12));
#4668=CARTESIAN_POINT('Origin',(0.11901961308292,6.21724893790088E-15,0.));
#4669=CARTESIAN_POINT('',(-0.868031252847412,0.633495422775111,0.));
#4670=CARTESIAN_POINT('Origin',(-0.947327569834341,0.493147518935016,0.));
#4671=CARTESIAN_POINT('Ctrl Pts',(-0.8680312528477,-0.633495422775274,0.));
#4672=CARTESIAN_POINT('Ctrl Pts',(-0.866468860926997,-0.635830722731769,
0.));
#4673=CARTESIAN_POINT('Ctrl Pts',(-0.861627881960007,-0.64301558066062,
0.));
#4674=CARTESIAN_POINT('Ctrl Pts',(-0.853391883864834,-0.654977418032855,
0.));
#4675=CARTESIAN_POINT('Ctrl Pts',(-0.841545334406876,-0.671576597784011,
0.));
#4676=CARTESIAN_POINT('Ctrl Pts',(-0.82578008117756,-0.69259659895799,0.));
#4677=CARTESIAN_POINT('Ctrl Pts',(-0.807540237001814,-0.715586030006588,
0.));
#4678=CARTESIAN_POINT('Ctrl Pts',(-0.788671222413511,-0.738083066750504,
0.));
#4679=CARTESIAN_POINT('Ctrl Pts',(-0.769188516988648,-0.760067206050057,
0.));
#4680=CARTESIAN_POINT('Ctrl Pts',(-0.749106566399864,-0.781521126617586,
0.));
#4681=CARTESIAN_POINT('Ctrl Pts',(-0.728439343631846,-0.802429621210541,
0.));
#4682=CARTESIAN_POINT('Ctrl Pts',(-0.707200722570354,-0.822778881439107,
0.));
#4683=CARTESIAN_POINT('Ctrl Pts',(-0.685404899341998,-0.84255569314248,
0.));
#4684=CARTESIAN_POINT('Ctrl Pts',(-0.663066855029994,-0.861746554484541,
0.));
#4685=CARTESIAN_POINT('Ctrl Pts',(-0.640202597886525,-0.880337207900968,
0.));
#4686=CARTESIAN_POINT('Ctrl Pts',(-0.61682888916888,-0.898313140761512,
0.));
#4687=CARTESIAN_POINT('Ctrl Pts',(-0.592963069825771,-0.915659897318245,
0.));
#4688=CARTESIAN_POINT('Ctrl Pts',(-0.568622860345861,-0.932363440835334,
0.));
#4689=CARTESIAN_POINT('Ctrl Pts',(-0.543826140229843,-0.948410555212658,
0.));
#4690=CARTESIAN_POINT('Ctrl Pts',(-0.518590849350175,-0.963789014835703,
0.));
#4691=CARTESIAN_POINT('Ctrl Pts',(-0.492935086995462,-0.978487378620622,
0.));
#4692=CARTESIAN_POINT('Ctrl Pts',(-0.466877166338143,-0.992494869297879,
0.));
#4693=CARTESIAN_POINT('Ctrl Pts',(-0.440435680606148,-1.00580123015714,
0.));
#4694=CARTESIAN_POINT('Ctrl Pts',(-0.413629579915119,-1.01839656305955,
0.));
#4695=CARTESIAN_POINT('Ctrl Pts',(-0.386478184359591,-1.03027128325725,
0.));
#4696=CARTESIAN_POINT('Ctrl Pts',(-0.359001120477101,-1.04141621492846,
0.));
#4697=CARTESIAN_POINT('Ctrl Pts',(-0.331218276777395,-1.05182265203972,
0.));
#4698=CARTESIAN_POINT('Ctrl Pts',(-0.30314975447047,-1.06148242804708,0.));
#4699=CARTESIAN_POINT('Ctrl Pts',(-0.2748158132226,-1.07038799540312,0.));
#4700=CARTESIAN_POINT('Ctrl Pts',(-0.246236848114779,-1.07853244619974,
0.));
#4701=CARTESIAN_POINT('Ctrl Pts',(-0.217433396017985,-1.08590947721852,
0.));
#4702=CARTESIAN_POINT('Ctrl Pts',(-0.188426134393584,-1.09251336987768,
0.));
#4703=CARTESIAN_POINT('Ctrl Pts',(-0.159235881741527,-1.09833896639077,
0.));
#4704=CARTESIAN_POINT('Ctrl Pts',(-0.129883601129733,-1.10338164243564,
0.));
#4705=CARTESIAN_POINT('Ctrl Pts',(-0.100390386189668,-1.1076373045706,0.));
#4706=CARTESIAN_POINT('Ctrl Pts',(-0.0707774336926613,-1.11110240713062,
0.));
#4707=CARTESIAN_POINT('Ctrl Pts',(-0.0410660195909007,-1.11377396404697,
0.));
#4708=CARTESIAN_POINT('Ctrl Pts',(-0.0112774747954127,-1.11564956182599,
0.));
#4709=CARTESIAN_POINT('Ctrl Pts',(0.0185668417359402,-1.11672737500119,
0.));
#4710=CARTESIAN_POINT('Ctrl Pts',(0.0484455558693415,-1.11700616793207,
0.));
#4711=CARTESIAN_POINT('Ctrl Pts',(0.0783372821756426,-1.11648528736655,
0.));
#4712=CARTESIAN_POINT('Ctrl Pts',(0.108220629786098,-1.11516465787405,0.));
#4713=CARTESIAN_POINT('Ctrl Pts',(0.138074209040328,-1.1130447764894,0.));
#4714=CARTESIAN_POINT('Ctrl Pts',(0.167876633777266,-1.11012670736124,0.));
#4715=CARTESIAN_POINT('Ctrl Pts',(0.197606544321918,-1.10641207905813,0.));
#4716=CARTESIAN_POINT('Ctrl Pts',(0.227242642150327,-1.10190308368776,0.));
#4717=CARTESIAN_POINT('Ctrl Pts',(0.256763722532457,-1.09660247571268,0.));
#4718=CARTESIAN_POINT('Ctrl Pts',(0.286148704656023,-1.09051357088032,0.));
#4719=CARTESIAN_POINT('Ctrl Pts',(0.315376671295726,-1.08364024578391,0.));
#4720=CARTESIAN_POINT('Ctrl Pts',(0.344426864523868,-1.07598693493533,0.));
#4721=CARTESIAN_POINT('Ctrl Pts',(0.373278657560889,-1.06755862629372,0.));
#4722=CARTESIAN_POINT('Ctrl Pts',(0.40191153059007,-1.05836085760139,0.));
#4723=CARTESIAN_POINT('Ctrl Pts',(0.430305052465067,-1.04839971220046,0.));
#4724=CARTESIAN_POINT('Ctrl Pts',(0.45843884125875,-1.03768181616585,0.));
#4725=CARTESIAN_POINT('Ctrl Pts',(0.486292621102405,-1.02621433076827,0.));
#4726=CARTESIAN_POINT('Ctrl Pts',(0.513846332693361,-1.01400494236352,0.));
#4727=CARTESIAN_POINT('Ctrl Pts',(0.541080235433912,-1.00106185298107,0.));
#4728=CARTESIAN_POINT('Ctrl Pts',(0.567974995595113,-0.987393771329312,
0.));
#4729=CARTESIAN_POINT('Ctrl Pts',(0.594511824092215,-0.973009902467593,
0.));
#4730=CARTESIAN_POINT('Ctrl Pts',(0.620672396673315,-0.957919944163756,
0.));
#4731=CARTESIAN_POINT('Ctrl Pts',(0.646438641619482,-0.942134087249009,
0.));
#4732=CARTESIAN_POINT('Ctrl Pts',(0.67179254905522,-0.925663015702513,0.));
#4733=CARTESIAN_POINT('Ctrl Pts',(0.696716011515847,-0.908517905290565,
0.));
#4734=CARTESIAN_POINT('Ctrl Pts',(0.721190552023322,-0.890710427237186,
0.));
#4735=CARTESIAN_POINT('Ctrl Pts',(0.745197525414791,-0.872252731655685,
0.));
#4736=CARTESIAN_POINT('Ctrl Pts',(0.768718652031186,-0.853157416735685,
0.));
#4737=CARTESIAN_POINT('Ctrl Pts',(0.791736496209353,-0.833437500599933,
0.));
#4738=CARTESIAN_POINT('Ctrl Pts',(0.814234876393174,-0.81310639575503,0.));
#4739=CARTESIAN_POINT('Ctrl Pts',(0.836199528793963,-0.792177873864096,
0.));
#4740=CARTESIAN_POINT('Ctrl Pts',(0.857617760934752,-0.770666069833932,
0.));
#4741=CARTESIAN_POINT('Ctrl Pts',(0.878477242115376,-0.74858551944097,0.));
#4742=CARTESIAN_POINT('Ctrl Pts',(0.898764943113291,-0.725951191437368,
0.));
#4743=CARTESIAN_POINT('Ctrl Pts',(0.918466214618678,-0.70277851394702,0.));
#4744=CARTESIAN_POINT('Ctrl Pts',(0.937563319582499,-0.679083423181946,
0.));
#4745=CARTESIAN_POINT('Ctrl Pts',(0.956036026761672,-0.654882328595489,
0.));
#4746=CARTESIAN_POINT('Ctrl Pts',(0.973864462863685,-0.630191986422907,
0.));
#4747=CARTESIAN_POINT('Ctrl Pts',(0.991031566790864,-0.605029389584474,
0.));
#4748=CARTESIAN_POINT('Ctrl Pts',(1.00752529081786,-0.579411667627393,0.));
#4749=CARTESIAN_POINT('Ctrl Pts',(1.02334191285221,-0.553355942423953,0.));
#4750=CARTESIAN_POINT('Ctrl Pts',(1.03848536635828,-0.526879343018338,0.));
#4751=CARTESIAN_POINT('Ctrl Pts',(1.05296063073153,-0.499999257829972,0.));
#4752=CARTESIAN_POINT('Ctrl Pts',(1.06676816041365,-0.472733545459157,0.));
#4753=CARTESIAN_POINT('Ctrl Pts',(1.0798986829592,-0.44510073074649,0.));
#4754=CARTESIAN_POINT('Ctrl Pts',(1.09232595504273,-0.417120282666841,0.));
#4755=CARTESIAN_POINT('Ctrl Pts',(1.1040065500515,-0.388812610728411,0.));
#4756=CARTESIAN_POINT('Ctrl Pts',(1.11489509573247,-0.360198442057814,0.));
#4757=CARTESIAN_POINT('Ctrl Pts',(1.12495696400084,-0.331298301519,0.));
#4758=CARTESIAN_POINT('Ctrl Pts',(1.13418071785862,-0.302131999517994,0.));
#4759=CARTESIAN_POINT('Ctrl Pts',(1.14259364432097,-0.272718001214759,0.));
#4760=CARTESIAN_POINT('Ctrl Pts',(1.15026681194464,-0.243073201156197,0.));
#4761=CARTESIAN_POINT('Ctrl Pts',(1.15728135528338,-0.213214209193066,0.));
#4762=CARTESIAN_POINT('Ctrl Pts',(1.16370031035361,-0.183158411923726,0.));
#4763=CARTESIAN_POINT('Ctrl Pts',(1.1695394362355,-0.152925093725504,0.));
#4764=CARTESIAN_POINT('Ctrl Pts',(1.17473573615846,-0.1225365994934,0.));
#4765=CARTESIAN_POINT('Ctrl Pts',(1.17912488557723,-0.0920192855934153,
0.));
#4766=CARTESIAN_POINT('Ctrl Pts',(1.18249458653374,-0.0614026081204919,
0.));
#4767=CARTESIAN_POINT('Ctrl Pts',(1.18463081328693,-0.0307183863950716,
0.));
#4768=CARTESIAN_POINT('Ctrl Pts',(1.18536679600018,3.34053531364509E-15,
0.));
#4769=CARTESIAN_POINT('Ctrl Pts',(1.18463081328694,0.0307183863950759,0.));
#4770=CARTESIAN_POINT('Ctrl Pts',(1.18249458653375,0.0614026081204918,0.));
#4771=CARTESIAN_POINT('Ctrl Pts',(1.17912488557725,0.0920192855934129,0.));
#4772=CARTESIAN_POINT('Ctrl Pts',(1.17473573615847,0.122536599493401,0.));
#4773=CARTESIAN_POINT('Ctrl Pts',(1.1695394362355,0.152925093725509,0.));
#4774=CARTESIAN_POINT('Ctrl Pts',(1.1637003103536,0.183158411923732,0.));
#4775=CARTESIAN_POINT('Ctrl Pts',(1.15728135528336,0.21321420919307,0.));
#4776=CARTESIAN_POINT('Ctrl Pts',(1.15026681194462,0.243073201156195,0.));
#4777=CARTESIAN_POINT('Ctrl Pts',(1.14259364432096,0.272718001214758,0.));
#4778=CARTESIAN_POINT('Ctrl Pts',(1.13418071785862,0.302131999517997,0.));
#4779=CARTESIAN_POINT('Ctrl Pts',(1.12495696400085,0.33129830151901,0.));
#4780=CARTESIAN_POINT('Ctrl Pts',(1.11489509573248,0.36019844205783,0.));
#4781=CARTESIAN_POINT('Ctrl Pts',(1.10400655005151,0.388812610728428,0.));
#4782=CARTESIAN_POINT('Ctrl Pts',(1.09232595504274,0.417120282666858,0.));
#4783=CARTESIAN_POINT('Ctrl Pts',(1.0798986829592,0.4451007307465,0.));
#4784=CARTESIAN_POINT('Ctrl Pts',(1.06676816041364,0.472733545459153,0.));
#4785=CARTESIAN_POINT('Ctrl Pts',(1.05296063073151,0.499999257829953,0.));
#4786=CARTESIAN_POINT('Ctrl Pts',(1.03848536635825,0.526879343018311,0.));
#4787=CARTESIAN_POINT('Ctrl Pts',(1.02334191285218,0.553355942423933,0.));
#4788=CARTESIAN_POINT('Ctrl Pts',(1.00752529081784,0.579411667627389,0.));
#4789=CARTESIAN_POINT('Ctrl Pts',(0.991031566790874,0.605029389584491,0.));
#4790=CARTESIAN_POINT('Ctrl Pts',(0.973864462863717,0.630191986422942,0.));
#4791=CARTESIAN_POINT('Ctrl Pts',(0.956036026761713,0.654882328595531,0.));
#4792=CARTESIAN_POINT('Ctrl Pts',(0.93756331958253,0.67908342318198,0.));
#4793=CARTESIAN_POINT('Ctrl Pts',(0.918466214618686,0.702778513947035,0.));
#4794=CARTESIAN_POINT('Ctrl Pts',(0.898764943113273,0.725951191437361,0.));
#4795=CARTESIAN_POINT('Ctrl Pts',(0.87847724211534,0.748585519440939,0.));
#4796=CARTESIAN_POINT('Ctrl Pts',(0.857617760934708,0.770666069833888,0.));
#4797=CARTESIAN_POINT('Ctrl Pts',(0.836199528793927,0.792177873864058,0.));
#4798=CARTESIAN_POINT('Ctrl Pts',(0.814234876393157,0.813106395755015,0.));
#4799=CARTESIAN_POINT('Ctrl Pts',(0.79173649620936,0.833437500599952,0.));
#4800=CARTESIAN_POINT('Ctrl Pts',(0.768718652031217,0.853157416735736,0.));
#4801=CARTESIAN_POINT('Ctrl Pts',(0.745197525414833,0.872252731655753,0.));
#4802=CARTESIAN_POINT('Ctrl Pts',(0.721190552023354,0.890710427237242,0.));
#4803=CARTESIAN_POINT('Ctrl Pts',(0.696716011515856,0.908517905290589,0.));
#4804=CARTESIAN_POINT('Ctrl Pts',(0.671792549055205,0.9256630157025,0.));
#4805=CARTESIAN_POINT('Ctrl Pts',(0.64643864161945,0.942134087248967,0.));
#4806=CARTESIAN_POINT('Ctrl Pts',(0.620672396673277,0.95791994416371,0.));
#4807=CARTESIAN_POINT('Ctrl Pts',(0.594511824092183,0.973009902467561,0.));
#4808=CARTESIAN_POINT('Ctrl Pts',(0.567974995595098,0.987393771329304,0.));
#4809=CARTESIAN_POINT('Ctrl Pts',(0.541080235433915,1.00106185298108,0.));
#4810=CARTESIAN_POINT('Ctrl Pts',(0.513846332693379,1.01400494236354,0.));
#4811=CARTESIAN_POINT('Ctrl Pts',(0.486292621102429,1.02621433076829,0.));
#4812=CARTESIAN_POINT('Ctrl Pts',(0.458438841258773,1.03768181616586,0.));
#4813=CARTESIAN_POINT('Ctrl Pts',(0.430305052465076,1.04839971220046,0.));
#4814=CARTESIAN_POINT('Ctrl Pts',(0.401911530590058,1.05836085760139,0.));
#4815=CARTESIAN_POINT('Ctrl Pts',(0.373278657560858,1.06755862629372,0.));
#4816=CARTESIAN_POINT('Ctrl Pts',(0.344426864523825,1.07598693493533,0.));
#4817=CARTESIAN_POINT('Ctrl Pts',(0.315376671295687,1.08364024578392,0.));
#4818=CARTESIAN_POINT('Ctrl Pts',(0.286148704656,1.09051357088032,0.));
#4819=CARTESIAN_POINT('Ctrl Pts',(0.256763722532462,1.09660247571268,0.));
#4820=CARTESIAN_POINT('Ctrl Pts',(0.22724264215036,1.10190308368774,0.));
#4821=CARTESIAN_POINT('Ctrl Pts',(0.197606544321966,1.10641207905811,0.));
#4822=CARTESIAN_POINT('Ctrl Pts',(0.167876633777302,1.11012670736122,0.));
#4823=CARTESIAN_POINT('Ctrl Pts',(0.138074209040338,1.11304477648939,0.));
#4824=CARTESIAN_POINT('Ctrl Pts',(0.108220629786082,1.11516465787406,0.));
#4825=CARTESIAN_POINT('Ctrl Pts',(0.0783372821756164,1.11648528736656,0.));
#4826=CARTESIAN_POINT('Ctrl Pts',(0.0484455558693182,1.11700616793208,0.));
#4827=CARTESIAN_POINT('Ctrl Pts',(0.0185668417359279,1.1167273750012,0.));
#4828=CARTESIAN_POINT('Ctrl Pts',(-0.011277474795416,1.11564956182599,0.));
#4829=CARTESIAN_POINT('Ctrl Pts',(-0.041066019590905,1.11377396404697,0.));
#4830=CARTESIAN_POINT('Ctrl Pts',(-0.0707774336926752,1.11110240713063,
0.));
#4831=CARTESIAN_POINT('Ctrl Pts',(-0.100390386189687,1.10763730457062,0.));
#4832=CARTESIAN_POINT('Ctrl Pts',(-0.129883601129753,1.10338164243566,0.));
#4833=CARTESIAN_POINT('Ctrl Pts',(-0.159235881741536,1.09833896639078,0.));
#4834=CARTESIAN_POINT('Ctrl Pts',(-0.188426134393585,1.09251336987768,0.));
#4835=CARTESIAN_POINT('Ctrl Pts',(-0.217433396017983,1.08590947721851,0.));
#4836=CARTESIAN_POINT('Ctrl Pts',(-0.246236848114778,1.07853244619972,0.));
#4837=CARTESIAN_POINT('Ctrl Pts',(-0.274815813222603,1.07038799540312,0.));
#4838=CARTESIAN_POINT('Ctrl Pts',(-0.303149754470475,1.06148242804708,0.));
#4839=CARTESIAN_POINT('Ctrl Pts',(-0.3312182767774,1.05182265203972,0.));
#4840=CARTESIAN_POINT('Ctrl Pts',(-0.359001120477101,1.04141621492845,0.));
#4841=CARTESIAN_POINT('Ctrl Pts',(-0.386478184359588,1.03027128325725,0.));
#4842=CARTESIAN_POINT('Ctrl Pts',(-0.413629579915113,1.01839656305955,0.));
#4843=CARTESIAN_POINT('Ctrl Pts',(-0.440435680606144,1.00580123015714,0.));
#4844=CARTESIAN_POINT('Ctrl Pts',(-0.466877166338154,0.992494869297873,
0.));
#4845=CARTESIAN_POINT('Ctrl Pts',(-0.492935086995497,0.97848737862061,0.));
#4846=CARTESIAN_POINT('Ctrl Pts',(-0.518590849350232,0.963789014835687,
0.));
#4847=CARTESIAN_POINT('Ctrl Pts',(-0.5438261402299,0.948410555212641,0.));
#4848=CARTESIAN_POINT('Ctrl Pts',(-0.568622860345892,0.932363440835325,
0.));
#4849=CARTESIAN_POINT('Ctrl Pts',(-0.592963069825743,0.91565989731825,0.));
#4850=CARTESIAN_POINT('Ctrl Pts',(-0.616828889168791,0.898313140761531,
0.));
#4851=CARTESIAN_POINT('Ctrl Pts',(-0.64020259788639,0.880337207900991,0.));
#4852=CARTESIAN_POINT('Ctrl Pts',(-0.663066855029865,0.861746554484547,
0.));
#4853=CARTESIAN_POINT('Ctrl Pts',(-0.685404899341948,0.842555693142475,
0.));
#4854=CARTESIAN_POINT('Ctrl Pts',(-0.707200722570447,0.822778881439102,
0.));
#4855=CARTESIAN_POINT('Ctrl Pts',(-0.728439343632102,0.802429621210551,
0.));
#4856=CARTESIAN_POINT('Ctrl Pts',(-0.749106566400217,0.781521126617609,
0.));
#4857=CARTESIAN_POINT('Ctrl Pts',(-0.76918851698896,0.760067206050081,0.));
#4858=CARTESIAN_POINT('Ctrl Pts',(-0.788671222413612,0.738083066750512,
0.));
#4859=CARTESIAN_POINT('Ctrl Pts',(-0.807540237001567,0.715586030006559,
0.));
#4860=CARTESIAN_POINT('Ctrl Pts',(-0.825780081176955,0.692596598957924,
0.));
#4861=CARTESIAN_POINT('Ctrl Pts',(-0.841545334406124,0.671576597783911,
0.));
#4862=CARTESIAN_POINT('Ctrl Pts',(-0.85339188386416,0.654977418032737,0.));
#4863=CARTESIAN_POINT('Ctrl Pts',(-0.861627881959507,0.643015580660492,
0.));
#4864=CARTESIAN_POINT('Ctrl Pts',(-0.866468860926645,0.635830722731627,
0.));
#4865=CARTESIAN_POINT('Ctrl Pts',(-0.868031252847412,0.633495422775111,
0.));
#4866=CARTESIAN_POINT('',(-1.04732756983434,0.493147518935016,0.));
#4867=CARTESIAN_POINT('Origin',(-0.947327569834341,0.493147518935016,0.));
#4868=CARTESIAN_POINT('',(-1.04732756983434,-0.493147518935016,0.));
#4869=CARTESIAN_POINT('Origin',(-0.947327569834341,-0.493147518935016,0.));
#4870=CARTESIAN_POINT('Origin',(-0.947327569834341,-0.493147518935016,0.));
#4871=CARTESIAN_POINT('',(-1.04732756983434,-0.493147518935016,0.12));
#4872=CARTESIAN_POINT('',(-1.04732756983434,-0.493147518935016,0.));
#4873=CARTESIAN_POINT('Origin',(-0.947327569834341,-0.493147518935016,0.12));
#4874=CARTESIAN_POINT('Origin',(-0.947327569834341,0.493147518935016,0.));
#4875=CARTESIAN_POINT('',(-1.04732756983434,0.493147518935016,0.12));
#4876=CARTESIAN_POINT('',(-1.04732756983434,0.493147518935016,0.));
#4877=CARTESIAN_POINT('Origin',(-0.947327569834341,0.493147518935016,0.12));
#4878=CARTESIAN_POINT('Origin',(-0.947327569834341,0.493147518935016,0.));
#4879=CARTESIAN_POINT('',(-0.868031252847412,0.633495422775111,0.12));
#4880=CARTESIAN_POINT('Origin',(-0.947327569834341,0.493147518935016,0.12));
#4881=CARTESIAN_POINT('Ctrl Pts',(-0.868031252847412,0.633495422775111,
0.));
#4882=CARTESIAN_POINT('Ctrl Pts',(-0.868031252847412,0.633495422775111,
0.02));
#4883=CARTESIAN_POINT('Ctrl Pts',(-0.868031252847412,0.633495422775111,
0.04));
#4884=CARTESIAN_POINT('Ctrl Pts',(-0.868031252847412,0.633495422775111,
0.08));
#4885=CARTESIAN_POINT('Ctrl Pts',(-0.868031252847412,0.633495422775111,
0.1));
#4886=CARTESIAN_POINT('Ctrl Pts',(-0.868031252847412,0.633495422775111,
0.12));
#4887=CARTESIAN_POINT('Ctrl Pts',(-0.947327569834341,-0.493147518935016,
0.));
#4888=CARTESIAN_POINT('Ctrl Pts',(-0.947327569834341,-0.493147518935016,
0.12));
#4889=CARTESIAN_POINT('Ctrl Pts',(-0.944839172148911,-0.49844797467551,
0.));
#4890=CARTESIAN_POINT('Ctrl Pts',(-0.944839172148911,-0.49844797467551,
0.12));
#4891=CARTESIAN_POINT('Ctrl Pts',(-0.939792491218341,-0.509010207622537,
0.));
#4892=CARTESIAN_POINT('Ctrl Pts',(-0.939792491218341,-0.509010207622537,
0.12));
#4893=CARTESIAN_POINT('Ctrl Pts',(-0.932012813069913,-0.524737521565753,
0.));
#4894=CARTESIAN_POINT('Ctrl Pts',(-0.932012813069913,-0.524737521565753,
0.12));
#4895=CARTESIAN_POINT('Ctrl Pts',(-0.921220578940944,-0.545475192012581,
0.));
#4896=CARTESIAN_POINT('Ctrl Pts',(-0.921220578940944,-0.545475192012581,
0.12));
#4897=CARTESIAN_POINT('Ctrl Pts',(-0.907032039302732,-0.571009280628982,
0.));
#4898=CARTESIAN_POINT('Ctrl Pts',(-0.907032039302732,-0.571009280628982,
0.12));
#4899=CARTESIAN_POINT('Ctrl Pts',(-0.892147344045788,-0.596151853069145,
0.));
#4900=CARTESIAN_POINT('Ctrl Pts',(-0.892147344045788,-0.596151853069145,
0.12));
#4901=CARTESIAN_POINT('Ctrl Pts',(-0.876570783334336,-0.620895981731386,
0.));
#4902=CARTESIAN_POINT('Ctrl Pts',(-0.876570783334336,-0.620895981731386,
0.12));
#4903=CARTESIAN_POINT('Ctrl Pts',(-0.860309667737524,-0.645230105165021,
0.));
#4904=CARTESIAN_POINT('Ctrl Pts',(-0.860309667737524,-0.645230105165021,
0.12));
#4905=CARTESIAN_POINT('Ctrl Pts',(-0.843374934437972,-0.669137170123564,
0.));
#4906=CARTESIAN_POINT('Ctrl Pts',(-0.843374934437972,-0.669137170123564,
0.12));
#4907=CARTESIAN_POINT('Ctrl Pts',(-0.82578008117756,-0.69259659895799,0.));
#4908=CARTESIAN_POINT('Ctrl Pts',(-0.82578008117756,-0.69259659895799,0.12));
#4909=CARTESIAN_POINT('Ctrl Pts',(-0.807540237001814,-0.715586030006588,
0.));
#4910=CARTESIAN_POINT('Ctrl Pts',(-0.807540237001814,-0.715586030006588,
0.12));
#4911=CARTESIAN_POINT('Ctrl Pts',(-0.788671222413511,-0.738083066750504,
0.));
#4912=CARTESIAN_POINT('Ctrl Pts',(-0.788671222413511,-0.738083066750504,
0.12));
#4913=CARTESIAN_POINT('Ctrl Pts',(-0.769188516988648,-0.760067206050057,
0.));
#4914=CARTESIAN_POINT('Ctrl Pts',(-0.769188516988648,-0.760067206050057,
0.12));
#4915=CARTESIAN_POINT('Ctrl Pts',(-0.749106566399864,-0.781521126617586,
0.));
#4916=CARTESIAN_POINT('Ctrl Pts',(-0.749106566399864,-0.781521126617586,
0.12));
#4917=CARTESIAN_POINT('Ctrl Pts',(-0.728439343631846,-0.802429621210541,
0.));
#4918=CARTESIAN_POINT('Ctrl Pts',(-0.728439343631846,-0.802429621210541,
0.12));
#4919=CARTESIAN_POINT('Ctrl Pts',(-0.707200722570354,-0.822778881439107,
0.));
#4920=CARTESIAN_POINT('Ctrl Pts',(-0.707200722570354,-0.822778881439107,
0.12));
#4921=CARTESIAN_POINT('Ctrl Pts',(-0.685404899341998,-0.84255569314248,
0.));
#4922=CARTESIAN_POINT('Ctrl Pts',(-0.685404899341998,-0.84255569314248,
0.12));
#4923=CARTESIAN_POINT('Ctrl Pts',(-0.663066855029994,-0.861746554484541,
0.));
#4924=CARTESIAN_POINT('Ctrl Pts',(-0.663066855029994,-0.861746554484541,
0.12));
#4925=CARTESIAN_POINT('Ctrl Pts',(-0.640202597886525,-0.880337207900968,
0.));
#4926=CARTESIAN_POINT('Ctrl Pts',(-0.640202597886525,-0.880337207900968,
0.12));
#4927=CARTESIAN_POINT('Ctrl Pts',(-0.61682888916888,-0.898313140761512,
0.));
#4928=CARTESIAN_POINT('Ctrl Pts',(-0.61682888916888,-0.898313140761512,
0.12));
#4929=CARTESIAN_POINT('Ctrl Pts',(-0.592963069825771,-0.915659897318245,
0.));
#4930=CARTESIAN_POINT('Ctrl Pts',(-0.592963069825771,-0.915659897318245,
0.12));
#4931=CARTESIAN_POINT('Ctrl Pts',(-0.568622860345861,-0.932363440835334,
0.));
#4932=CARTESIAN_POINT('Ctrl Pts',(-0.568622860345861,-0.932363440835334,
0.12));
#4933=CARTESIAN_POINT('Ctrl Pts',(-0.543826140229843,-0.948410555212658,
0.));
#4934=CARTESIAN_POINT('Ctrl Pts',(-0.543826140229843,-0.948410555212658,
0.12));
#4935=CARTESIAN_POINT('Ctrl Pts',(-0.518590849350175,-0.963789014835703,
0.));
#4936=CARTESIAN_POINT('Ctrl Pts',(-0.518590849350175,-0.963789014835703,
0.12));
#4937=CARTESIAN_POINT('Ctrl Pts',(-0.492935086995462,-0.978487378620622,
0.));
#4938=CARTESIAN_POINT('Ctrl Pts',(-0.492935086995462,-0.978487378620622,
0.12));
#4939=CARTESIAN_POINT('Ctrl Pts',(-0.466877166338143,-0.992494869297879,
0.));
#4940=CARTESIAN_POINT('Ctrl Pts',(-0.466877166338143,-0.992494869297879,
0.12));
#4941=CARTESIAN_POINT('Ctrl Pts',(-0.440435680606148,-1.00580123015714,
0.));
#4942=CARTESIAN_POINT('Ctrl Pts',(-0.440435680606148,-1.00580123015714,
0.12));
#4943=CARTESIAN_POINT('Ctrl Pts',(-0.413629579915119,-1.01839656305955,
0.));
#4944=CARTESIAN_POINT('Ctrl Pts',(-0.413629579915119,-1.01839656305955,
0.12));
#4945=CARTESIAN_POINT('Ctrl Pts',(-0.386478184359591,-1.03027128325725,
0.));
#4946=CARTESIAN_POINT('Ctrl Pts',(-0.386478184359591,-1.03027128325725,
0.12));
#4947=CARTESIAN_POINT('Ctrl Pts',(-0.359001120477101,-1.04141621492846,
0.));
#4948=CARTESIAN_POINT('Ctrl Pts',(-0.359001120477101,-1.04141621492846,
0.12));
#4949=CARTESIAN_POINT('Ctrl Pts',(-0.331218276777395,-1.05182265203972,
0.));
#4950=CARTESIAN_POINT('Ctrl Pts',(-0.331218276777395,-1.05182265203972,
0.12));
#4951=CARTESIAN_POINT('Ctrl Pts',(-0.30314975447047,-1.06148242804708,0.));
#4952=CARTESIAN_POINT('Ctrl Pts',(-0.30314975447047,-1.06148242804708,0.12));
#4953=CARTESIAN_POINT('Ctrl Pts',(-0.2748158132226,-1.07038799540312,0.));
#4954=CARTESIAN_POINT('Ctrl Pts',(-0.2748158132226,-1.07038799540312,0.12));
#4955=CARTESIAN_POINT('Ctrl Pts',(-0.246236848114779,-1.07853244619974,
0.));
#4956=CARTESIAN_POINT('Ctrl Pts',(-0.246236848114779,-1.07853244619974,
0.12));
#4957=CARTESIAN_POINT('Ctrl Pts',(-0.217433396017985,-1.08590947721852,
0.));
#4958=CARTESIAN_POINT('Ctrl Pts',(-0.217433396017985,-1.08590947721852,
0.12));
#4959=CARTESIAN_POINT('Ctrl Pts',(-0.188426134393584,-1.09251336987768,
0.));
#4960=CARTESIAN_POINT('Ctrl Pts',(-0.188426134393584,-1.09251336987768,
0.12));
#4961=CARTESIAN_POINT('Ctrl Pts',(-0.159235881741527,-1.09833896639077,
0.));
#4962=CARTESIAN_POINT('Ctrl Pts',(-0.159235881741527,-1.09833896639077,
0.12));
#4963=CARTESIAN_POINT('Ctrl Pts',(-0.129883601129733,-1.10338164243564,
0.));
#4964=CARTESIAN_POINT('Ctrl Pts',(-0.129883601129733,-1.10338164243564,
0.12));
#4965=CARTESIAN_POINT('Ctrl Pts',(-0.100390386189668,-1.1076373045706,0.));
#4966=CARTESIAN_POINT('Ctrl Pts',(-0.100390386189668,-1.1076373045706,0.12));
#4967=CARTESIAN_POINT('Ctrl Pts',(-0.0707774336926613,-1.11110240713062,
0.));
#4968=CARTESIAN_POINT('Ctrl Pts',(-0.0707774336926613,-1.11110240713062,
0.12));
#4969=CARTESIAN_POINT('Ctrl Pts',(-0.0410660195909007,-1.11377396404697,
0.));
#4970=CARTESIAN_POINT('Ctrl Pts',(-0.0410660195909007,-1.11377396404697,
0.12));
#4971=CARTESIAN_POINT('Ctrl Pts',(-0.0112774747954127,-1.11564956182599,
0.));
#4972=CARTESIAN_POINT('Ctrl Pts',(-0.0112774747954127,-1.11564956182599,
0.12));
#4973=CARTESIAN_POINT('Ctrl Pts',(0.0185668417359402,-1.11672737500119,
0.));
#4974=CARTESIAN_POINT('Ctrl Pts',(0.0185668417359402,-1.11672737500119,
0.12));
#4975=CARTESIAN_POINT('Ctrl Pts',(0.0484455558693415,-1.11700616793207,
0.));
#4976=CARTESIAN_POINT('Ctrl Pts',(0.0484455558693415,-1.11700616793207,
0.12));
#4977=CARTESIAN_POINT('Ctrl Pts',(0.0783372821756426,-1.11648528736655,
0.));
#4978=CARTESIAN_POINT('Ctrl Pts',(0.0783372821756426,-1.11648528736655,
0.12));
#4979=CARTESIAN_POINT('Ctrl Pts',(0.108220629786098,-1.11516465787405,0.));
#4980=CARTESIAN_POINT('Ctrl Pts',(0.108220629786098,-1.11516465787405,0.12));
#4981=CARTESIAN_POINT('Ctrl Pts',(0.138074209040328,-1.1130447764894,0.));
#4982=CARTESIAN_POINT('Ctrl Pts',(0.138074209040328,-1.1130447764894,0.12));
#4983=CARTESIAN_POINT('Ctrl Pts',(0.167876633777266,-1.11012670736124,0.));
#4984=CARTESIAN_POINT('Ctrl Pts',(0.167876633777266,-1.11012670736124,0.12));
#4985=CARTESIAN_POINT('Ctrl Pts',(0.197606544321918,-1.10641207905813,0.));
#4986=CARTESIAN_POINT('Ctrl Pts',(0.197606544321918,-1.10641207905813,0.12));
#4987=CARTESIAN_POINT('Ctrl Pts',(0.227242642150327,-1.10190308368776,0.));
#4988=CARTESIAN_POINT('Ctrl Pts',(0.227242642150327,-1.10190308368776,0.12));
#4989=CARTESIAN_POINT('Ctrl Pts',(0.256763722532457,-1.09660247571268,0.));
#4990=CARTESIAN_POINT('Ctrl Pts',(0.256763722532457,-1.09660247571268,0.12));
#4991=CARTESIAN_POINT('Ctrl Pts',(0.286148704656023,-1.09051357088032,0.));
#4992=CARTESIAN_POINT('Ctrl Pts',(0.286148704656023,-1.09051357088032,0.12));
#4993=CARTESIAN_POINT('Ctrl Pts',(0.315376671295726,-1.08364024578391,0.));
#4994=CARTESIAN_POINT('Ctrl Pts',(0.315376671295726,-1.08364024578391,0.12));
#4995=CARTESIAN_POINT('Ctrl Pts',(0.344426864523868,-1.07598693493533,0.));
#4996=CARTESIAN_POINT('Ctrl Pts',(0.344426864523868,-1.07598693493533,0.12));
#4997=CARTESIAN_POINT('Ctrl Pts',(0.373278657560889,-1.06755862629372,0.));
#4998=CARTESIAN_POINT('Ctrl Pts',(0.373278657560889,-1.06755862629372,0.12));
#4999=CARTESIAN_POINT('Ctrl Pts',(0.40191153059007,-1.05836085760139,0.));
#5000=CARTESIAN_POINT('Ctrl Pts',(0.40191153059007,-1.05836085760139,0.12));
#5001=CARTESIAN_POINT('Ctrl Pts',(0.430305052465067,-1.04839971220046,0.));
#5002=CARTESIAN_POINT('Ctrl Pts',(0.430305052465067,-1.04839971220046,0.12));
#5003=CARTESIAN_POINT('Ctrl Pts',(0.45843884125875,-1.03768181616585,0.));
#5004=CARTESIAN_POINT('Ctrl Pts',(0.45843884125875,-1.03768181616585,0.12));
#5005=CARTESIAN_POINT('Ctrl Pts',(0.486292621102405,-1.02621433076827,0.));
#5006=CARTESIAN_POINT('Ctrl Pts',(0.486292621102405,-1.02621433076827,0.12));
#5007=CARTESIAN_POINT('Ctrl Pts',(0.513846332693361,-1.01400494236352,0.));
#5008=CARTESIAN_POINT('Ctrl Pts',(0.513846332693361,-1.01400494236352,0.12));
#5009=CARTESIAN_POINT('Ctrl Pts',(0.541080235433912,-1.00106185298107,0.));
#5010=CARTESIAN_POINT('Ctrl Pts',(0.541080235433912,-1.00106185298107,0.12));
#5011=CARTESIAN_POINT('Ctrl Pts',(0.567974995595113,-0.987393771329312,
0.));
#5012=CARTESIAN_POINT('Ctrl Pts',(0.567974995595113,-0.987393771329312,
0.12));
#5013=CARTESIAN_POINT('Ctrl Pts',(0.594511824092215,-0.973009902467593,
0.));
#5014=CARTESIAN_POINT('Ctrl Pts',(0.594511824092215,-0.973009902467593,
0.12));
#5015=CARTESIAN_POINT('Ctrl Pts',(0.620672396673315,-0.957919944163756,
0.));
#5016=CARTESIAN_POINT('Ctrl Pts',(0.620672396673315,-0.957919944163756,
0.12));
#5017=CARTESIAN_POINT('Ctrl Pts',(0.646438641619482,-0.942134087249009,
0.));
#5018=CARTESIAN_POINT('Ctrl Pts',(0.646438641619482,-0.942134087249009,
0.12));
#5019=CARTESIAN_POINT('Ctrl Pts',(0.67179254905522,-0.925663015702513,0.));
#5020=CARTESIAN_POINT('Ctrl Pts',(0.67179254905522,-0.925663015702513,0.12));
#5021=CARTESIAN_POINT('Ctrl Pts',(0.696716011515847,-0.908517905290565,
0.));
#5022=CARTESIAN_POINT('Ctrl Pts',(0.696716011515847,-0.908517905290565,
0.12));
#5023=CARTESIAN_POINT('Ctrl Pts',(0.721190552023322,-0.890710427237186,
0.));
#5024=CARTESIAN_POINT('Ctrl Pts',(0.721190552023322,-0.890710427237186,
0.12));
#5025=CARTESIAN_POINT('Ctrl Pts',(0.745197525414791,-0.872252731655685,
0.));
#5026=CARTESIAN_POINT('Ctrl Pts',(0.745197525414791,-0.872252731655685,
0.12));
#5027=CARTESIAN_POINT('Ctrl Pts',(0.768718652031186,-0.853157416735685,
0.));
#5028=CARTESIAN_POINT('Ctrl Pts',(0.768718652031186,-0.853157416735685,
0.12));
#5029=CARTESIAN_POINT('Ctrl Pts',(0.791736496209353,-0.833437500599933,
0.));
#5030=CARTESIAN_POINT('Ctrl Pts',(0.791736496209353,-0.833437500599933,
0.12));
#5031=CARTESIAN_POINT('Ctrl Pts',(0.814234876393174,-0.81310639575503,0.));
#5032=CARTESIAN_POINT('Ctrl Pts',(0.814234876393174,-0.81310639575503,0.12));
#5033=CARTESIAN_POINT('Ctrl Pts',(0.836199528793963,-0.792177873864096,
0.));
#5034=CARTESIAN_POINT('Ctrl Pts',(0.836199528793963,-0.792177873864096,
0.12));
#5035=CARTESIAN_POINT('Ctrl Pts',(0.857617760934752,-0.770666069833932,
0.));
#5036=CARTESIAN_POINT('Ctrl Pts',(0.857617760934752,-0.770666069833932,
0.12));
#5037=CARTESIAN_POINT('Ctrl Pts',(0.878477242115376,-0.74858551944097,0.));
#5038=CARTESIAN_POINT('Ctrl Pts',(0.878477242115376,-0.74858551944097,0.12));
#5039=CARTESIAN_POINT('Ctrl Pts',(0.898764943113291,-0.725951191437368,
0.));
#5040=CARTESIAN_POINT('Ctrl Pts',(0.898764943113291,-0.725951191437368,
0.12));
#5041=CARTESIAN_POINT('Ctrl Pts',(0.918466214618678,-0.70277851394702,0.));
#5042=CARTESIAN_POINT('Ctrl Pts',(0.918466214618678,-0.70277851394702,0.12));
#5043=CARTESIAN_POINT('Ctrl Pts',(0.937563319582499,-0.679083423181946,
0.));
#5044=CARTESIAN_POINT('Ctrl Pts',(0.937563319582499,-0.679083423181946,
0.12));
#5045=CARTESIAN_POINT('Ctrl Pts',(0.956036026761672,-0.654882328595489,
0.));
#5046=CARTESIAN_POINT('Ctrl Pts',(0.956036026761672,-0.654882328595489,
0.12));
#5047=CARTESIAN_POINT('Ctrl Pts',(0.973864462863685,-0.630191986422907,
0.));
#5048=CARTESIAN_POINT('Ctrl Pts',(0.973864462863685,-0.630191986422907,
0.12));
#5049=CARTESIAN_POINT('Ctrl Pts',(0.991031566790864,-0.605029389584474,
0.));
#5050=CARTESIAN_POINT('Ctrl Pts',(0.991031566790864,-0.605029389584474,
0.12));
#5051=CARTESIAN_POINT('Ctrl Pts',(1.00752529081786,-0.579411667627393,0.));
#5052=CARTESIAN_POINT('Ctrl Pts',(1.00752529081786,-0.579411667627393,0.12));
#5053=CARTESIAN_POINT('Ctrl Pts',(1.02334191285221,-0.553355942423953,0.));
#5054=CARTESIAN_POINT('Ctrl Pts',(1.02334191285221,-0.553355942423953,0.12));
#5055=CARTESIAN_POINT('Ctrl Pts',(1.03848536635828,-0.526879343018338,0.));
#5056=CARTESIAN_POINT('Ctrl Pts',(1.03848536635828,-0.526879343018338,0.12));
#5057=CARTESIAN_POINT('Ctrl Pts',(1.05296063073153,-0.499999257829972,0.));
#5058=CARTESIAN_POINT('Ctrl Pts',(1.05296063073153,-0.499999257829972,0.12));
#5059=CARTESIAN_POINT('Ctrl Pts',(1.06676816041365,-0.472733545459157,0.));
#5060=CARTESIAN_POINT('Ctrl Pts',(1.06676816041365,-0.472733545459157,0.12));
#5061=CARTESIAN_POINT('Ctrl Pts',(1.0798986829592,-0.44510073074649,0.));
#5062=CARTESIAN_POINT('Ctrl Pts',(1.0798986829592,-0.44510073074649,0.12));
#5063=CARTESIAN_POINT('Ctrl Pts',(1.09232595504273,-0.417120282666841,0.));
#5064=CARTESIAN_POINT('Ctrl Pts',(1.09232595504273,-0.417120282666841,0.12));
#5065=CARTESIAN_POINT('Ctrl Pts',(1.1040065500515,-0.388812610728411,0.));
#5066=CARTESIAN_POINT('Ctrl Pts',(1.1040065500515,-0.388812610728411,0.12));
#5067=CARTESIAN_POINT('Ctrl Pts',(1.11489509573247,-0.360198442057814,0.));
#5068=CARTESIAN_POINT('Ctrl Pts',(1.11489509573247,-0.360198442057814,0.12));
#5069=CARTESIAN_POINT('Ctrl Pts',(1.12495696400084,-0.331298301519,0.));
#5070=CARTESIAN_POINT('Ctrl Pts',(1.12495696400084,-0.331298301519,0.12));
#5071=CARTESIAN_POINT('Ctrl Pts',(1.13418071785862,-0.302131999517994,0.));
#5072=CARTESIAN_POINT('Ctrl Pts',(1.13418071785862,-0.302131999517994,0.12));
#5073=CARTESIAN_POINT('Ctrl Pts',(1.14259364432097,-0.272718001214759,0.));
#5074=CARTESIAN_POINT('Ctrl Pts',(1.14259364432097,-0.272718001214759,0.12));
#5075=CARTESIAN_POINT('Ctrl Pts',(1.15026681194464,-0.243073201156197,0.));
#5076=CARTESIAN_POINT('Ctrl Pts',(1.15026681194464,-0.243073201156197,0.12));
#5077=CARTESIAN_POINT('Ctrl Pts',(1.15728135528338,-0.213214209193066,0.));
#5078=CARTESIAN_POINT('Ctrl Pts',(1.15728135528338,-0.213214209193066,0.12));
#5079=CARTESIAN_POINT('Ctrl Pts',(1.16370031035361,-0.183158411923726,0.));
#5080=CARTESIAN_POINT('Ctrl Pts',(1.16370031035361,-0.183158411923726,0.12));
#5081=CARTESIAN_POINT('Ctrl Pts',(1.1695394362355,-0.152925093725504,0.));
#5082=CARTESIAN_POINT('Ctrl Pts',(1.1695394362355,-0.152925093725504,0.12));
#5083=CARTESIAN_POINT('Ctrl Pts',(1.17473573615846,-0.1225365994934,0.));
#5084=CARTESIAN_POINT('Ctrl Pts',(1.17473573615846,-0.1225365994934,0.12));
#5085=CARTESIAN_POINT('Ctrl Pts',(1.17912488557723,-0.0920192855934153,
0.));
#5086=CARTESIAN_POINT('Ctrl Pts',(1.17912488557723,-0.0920192855934153,
0.12));
#5087=CARTESIAN_POINT('Ctrl Pts',(1.18249458653374,-0.0614026081204919,
0.));
#5088=CARTESIAN_POINT('Ctrl Pts',(1.18249458653374,-0.0614026081204919,
0.12));
#5089=CARTESIAN_POINT('Ctrl Pts',(1.18463081328693,-0.0307183863950716,
0.));
#5090=CARTESIAN_POINT('Ctrl Pts',(1.18463081328693,-0.0307183863950716,
0.12));
#5091=CARTESIAN_POINT('Ctrl Pts',(1.18536679600018,3.34053531364509E-15,
0.));
#5092=CARTESIAN_POINT('Ctrl Pts',(1.18536679600018,3.34053531364509E-15,
0.12));
#5093=CARTESIAN_POINT('Ctrl Pts',(1.18463081328694,0.0307183863950759,0.));
#5094=CARTESIAN_POINT('Ctrl Pts',(1.18463081328694,0.0307183863950759,0.12));
#5095=CARTESIAN_POINT('Ctrl Pts',(1.18249458653375,0.0614026081204918,0.));
#5096=CARTESIAN_POINT('Ctrl Pts',(1.18249458653375,0.0614026081204918,0.12));
#5097=CARTESIAN_POINT('Ctrl Pts',(1.17912488557725,0.0920192855934129,0.));
#5098=CARTESIAN_POINT('Ctrl Pts',(1.17912488557725,0.0920192855934129,0.12));
#5099=CARTESIAN_POINT('Ctrl Pts',(1.17473573615847,0.122536599493401,0.));
#5100=CARTESIAN_POINT('Ctrl Pts',(1.17473573615847,0.122536599493401,0.12));
#5101=CARTESIAN_POINT('Ctrl Pts',(1.1695394362355,0.152925093725509,0.));
#5102=CARTESIAN_POINT('Ctrl Pts',(1.1695394362355,0.152925093725509,0.12));
#5103=CARTESIAN_POINT('Ctrl Pts',(1.1637003103536,0.183158411923732,0.));
#5104=CARTESIAN_POINT('Ctrl Pts',(1.1637003103536,0.183158411923732,0.12));
#5105=CARTESIAN_POINT('Ctrl Pts',(1.15728135528336,0.21321420919307,0.));
#5106=CARTESIAN_POINT('Ctrl Pts',(1.15728135528336,0.21321420919307,0.12));
#5107=CARTESIAN_POINT('Ctrl Pts',(1.15026681194462,0.243073201156195,0.));
#5108=CARTESIAN_POINT('Ctrl Pts',(1.15026681194462,0.243073201156195,0.12));
#5109=CARTESIAN_POINT('Ctrl Pts',(1.14259364432096,0.272718001214758,0.));
#5110=CARTESIAN_POINT('Ctrl Pts',(1.14259364432096,0.272718001214758,0.12));
#5111=CARTESIAN_POINT('Ctrl Pts',(1.13418071785862,0.302131999517997,0.));
#5112=CARTESIAN_POINT('Ctrl Pts',(1.13418071785862,0.302131999517997,0.12));
#5113=CARTESIAN_POINT('Ctrl Pts',(1.12495696400085,0.33129830151901,0.));
#5114=CARTESIAN_POINT('Ctrl Pts',(1.12495696400085,0.33129830151901,0.12));
#5115=CARTESIAN_POINT('Ctrl Pts',(1.11489509573248,0.36019844205783,0.));
#5116=CARTESIAN_POINT('Ctrl Pts',(1.11489509573248,0.36019844205783,0.12));
#5117=CARTESIAN_POINT('Ctrl Pts',(1.10400655005151,0.388812610728428,0.));
#5118=CARTESIAN_POINT('Ctrl Pts',(1.10400655005151,0.388812610728428,0.12));
#5119=CARTESIAN_POINT('Ctrl Pts',(1.09232595504274,0.417120282666858,0.));
#5120=CARTESIAN_POINT('Ctrl Pts',(1.09232595504274,0.417120282666858,0.12));
#5121=CARTESIAN_POINT('Ctrl Pts',(1.0798986829592,0.4451007307465,0.));
#5122=CARTESIAN_POINT('Ctrl Pts',(1.0798986829592,0.4451007307465,0.12));
#5123=CARTESIAN_POINT('Ctrl Pts',(1.06676816041364,0.472733545459153,0.));
#5124=CARTESIAN_POINT('Ctrl Pts',(1.06676816041364,0.472733545459153,0.12));
#5125=CARTESIAN_POINT('Ctrl Pts',(1.05296063073151,0.499999257829953,0.));
#5126=CARTESIAN_POINT('Ctrl Pts',(1.05296063073151,0.499999257829953,0.12));
#5127=CARTESIAN_POINT('Ctrl Pts',(1.03848536635825,0.526879343018311,0.));
#5128=CARTESIAN_POINT('Ctrl Pts',(1.03848536635825,0.526879343018311,0.12));
#5129=CARTESIAN_POINT('Ctrl Pts',(1.02334191285218,0.553355942423933,0.));
#5130=CARTESIAN_POINT('Ctrl Pts',(1.02334191285218,0.553355942423933,0.12));
#5131=CARTESIAN_POINT('Ctrl Pts',(1.00752529081784,0.579411667627389,0.));
#5132=CARTESIAN_POINT('Ctrl Pts',(1.00752529081784,0.579411667627389,0.12));
#5133=CARTESIAN_POINT('Ctrl Pts',(0.991031566790874,0.605029389584491,0.));
#5134=CARTESIAN_POINT('Ctrl Pts',(0.991031566790874,0.605029389584491,0.12));
#5135=CARTESIAN_POINT('Ctrl Pts',(0.973864462863717,0.630191986422942,0.));
#5136=CARTESIAN_POINT('Ctrl Pts',(0.973864462863717,0.630191986422942,0.12));
#5137=CARTESIAN_POINT('Ctrl Pts',(0.956036026761713,0.654882328595531,0.));
#5138=CARTESIAN_POINT('Ctrl Pts',(0.956036026761713,0.654882328595531,0.12));
#5139=CARTESIAN_POINT('Ctrl Pts',(0.93756331958253,0.67908342318198,0.));
#5140=CARTESIAN_POINT('Ctrl Pts',(0.93756331958253,0.67908342318198,0.12));
#5141=CARTESIAN_POINT('Ctrl Pts',(0.918466214618686,0.702778513947035,0.));
#5142=CARTESIAN_POINT('Ctrl Pts',(0.918466214618686,0.702778513947035,0.12));
#5143=CARTESIAN_POINT('Ctrl Pts',(0.898764943113273,0.725951191437361,0.));
#5144=CARTESIAN_POINT('Ctrl Pts',(0.898764943113273,0.725951191437361,0.12));
#5145=CARTESIAN_POINT('Ctrl Pts',(0.87847724211534,0.748585519440939,0.));
#5146=CARTESIAN_POINT('Ctrl Pts',(0.87847724211534,0.748585519440939,0.12));
#5147=CARTESIAN_POINT('Ctrl Pts',(0.857617760934708,0.770666069833888,0.));
#5148=CARTESIAN_POINT('Ctrl Pts',(0.857617760934708,0.770666069833888,0.12));
#5149=CARTESIAN_POINT('Ctrl Pts',(0.836199528793927,0.792177873864058,0.));
#5150=CARTESIAN_POINT('Ctrl Pts',(0.836199528793927,0.792177873864058,0.12));
#5151=CARTESIAN_POINT('Ctrl Pts',(0.814234876393157,0.813106395755015,0.));
#5152=CARTESIAN_POINT('Ctrl Pts',(0.814234876393157,0.813106395755015,0.12));
#5153=CARTESIAN_POINT('Ctrl Pts',(0.79173649620936,0.833437500599952,0.));
#5154=CARTESIAN_POINT('Ctrl Pts',(0.79173649620936,0.833437500599952,0.12));
#5155=CARTESIAN_POINT('Ctrl Pts',(0.768718652031217,0.853157416735736,0.));
#5156=CARTESIAN_POINT('Ctrl Pts',(0.768718652031217,0.853157416735736,0.12));
#5157=CARTESIAN_POINT('Ctrl Pts',(0.745197525414833,0.872252731655753,0.));
#5158=CARTESIAN_POINT('Ctrl Pts',(0.745197525414833,0.872252731655753,0.12));
#5159=CARTESIAN_POINT('Ctrl Pts',(0.721190552023354,0.890710427237242,0.));
#5160=CARTESIAN_POINT('Ctrl Pts',(0.721190552023354,0.890710427237242,0.12));
#5161=CARTESIAN_POINT('Ctrl Pts',(0.696716011515856,0.908517905290589,0.));
#5162=CARTESIAN_POINT('Ctrl Pts',(0.696716011515856,0.908517905290589,0.12));
#5163=CARTESIAN_POINT('Ctrl Pts',(0.671792549055205,0.9256630157025,0.));
#5164=CARTESIAN_POINT('Ctrl Pts',(0.671792549055205,0.9256630157025,0.12));
#5165=CARTESIAN_POINT('Ctrl Pts',(0.64643864161945,0.942134087248967,0.));
#5166=CARTESIAN_POINT('Ctrl Pts',(0.64643864161945,0.942134087248967,0.12));
#5167=CARTESIAN_POINT('Ctrl Pts',(0.620672396673277,0.95791994416371,0.));
#5168=CARTESIAN_POINT('Ctrl Pts',(0.620672396673277,0.95791994416371,0.12));
#5169=CARTESIAN_POINT('Ctrl Pts',(0.594511824092183,0.973009902467561,0.));
#5170=CARTESIAN_POINT('Ctrl Pts',(0.594511824092183,0.973009902467561,0.12));
#5171=CARTESIAN_POINT('Ctrl Pts',(0.567974995595098,0.987393771329304,0.));
#5172=CARTESIAN_POINT('Ctrl Pts',(0.567974995595098,0.987393771329304,0.12));
#5173=CARTESIAN_POINT('Ctrl Pts',(0.541080235433915,1.00106185298108,0.));
#5174=CARTESIAN_POINT('Ctrl Pts',(0.541080235433915,1.00106185298108,0.12));
#5175=CARTESIAN_POINT('Ctrl Pts',(0.513846332693379,1.01400494236354,0.));
#5176=CARTESIAN_POINT('Ctrl Pts',(0.513846332693379,1.01400494236354,0.12));
#5177=CARTESIAN_POINT('Ctrl Pts',(0.486292621102429,1.02621433076829,0.));
#5178=CARTESIAN_POINT('Ctrl Pts',(0.486292621102429,1.02621433076829,0.12));
#5179=CARTESIAN_POINT('Ctrl Pts',(0.458438841258773,1.03768181616586,0.));
#5180=CARTESIAN_POINT('Ctrl Pts',(0.458438841258773,1.03768181616586,0.12));
#5181=CARTESIAN_POINT('Ctrl Pts',(0.430305052465076,1.04839971220046,0.));
#5182=CARTESIAN_POINT('Ctrl Pts',(0.430305052465076,1.04839971220046,0.12));
#5183=CARTESIAN_POINT('Ctrl Pts',(0.401911530590058,1.05836085760139,0.));
#5184=CARTESIAN_POINT('Ctrl Pts',(0.401911530590058,1.05836085760139,0.12));
#5185=CARTESIAN_POINT('Ctrl Pts',(0.373278657560858,1.06755862629372,0.));
#5186=CARTESIAN_POINT('Ctrl Pts',(0.373278657560858,1.06755862629372,0.12));
#5187=CARTESIAN_POINT('Ctrl Pts',(0.344426864523825,1.07598693493533,0.));
#5188=CARTESIAN_POINT('Ctrl Pts',(0.344426864523825,1.07598693493533,0.12));
#5189=CARTESIAN_POINT('Ctrl Pts',(0.315376671295687,1.08364024578392,0.));
#5190=CARTESIAN_POINT('Ctrl Pts',(0.315376671295687,1.08364024578392,0.12));
#5191=CARTESIAN_POINT('Ctrl Pts',(0.286148704656,1.09051357088032,0.));
#5192=CARTESIAN_POINT('Ctrl Pts',(0.286148704656,1.09051357088032,0.12));
#5193=CARTESIAN_POINT('Ctrl Pts',(0.256763722532462,1.09660247571268,0.));
#5194=CARTESIAN_POINT('Ctrl Pts',(0.256763722532462,1.09660247571268,0.12));
#5195=CARTESIAN_POINT('Ctrl Pts',(0.22724264215036,1.10190308368774,0.));
#5196=CARTESIAN_POINT('Ctrl Pts',(0.22724264215036,1.10190308368774,0.12));
#5197=CARTESIAN_POINT('Ctrl Pts',(0.197606544321966,1.10641207905811,0.));
#5198=CARTESIAN_POINT('Ctrl Pts',(0.197606544321966,1.10641207905811,0.12));
#5199=CARTESIAN_POINT('Ctrl Pts',(0.167876633777302,1.11012670736122,0.));
#5200=CARTESIAN_POINT('Ctrl Pts',(0.167876633777302,1.11012670736122,0.12));
#5201=CARTESIAN_POINT('Ctrl Pts',(0.138074209040338,1.11304477648939,0.));
#5202=CARTESIAN_POINT('Ctrl Pts',(0.138074209040338,1.11304477648939,0.12));
#5203=CARTESIAN_POINT('Ctrl Pts',(0.108220629786082,1.11516465787406,0.));
#5204=CARTESIAN_POINT('Ctrl Pts',(0.108220629786082,1.11516465787406,0.12));
#5205=CARTESIAN_POINT('Ctrl Pts',(0.0783372821756164,1.11648528736656,0.));
#5206=CARTESIAN_POINT('Ctrl Pts',(0.0783372821756164,1.11648528736656,0.12));
#5207=CARTESIAN_POINT('Ctrl Pts',(0.0484455558693182,1.11700616793208,0.));
#5208=CARTESIAN_POINT('Ctrl Pts',(0.0484455558693182,1.11700616793208,0.12));
#5209=CARTESIAN_POINT('Ctrl Pts',(0.0185668417359279,1.1167273750012,0.));
#5210=CARTESIAN_POINT('Ctrl Pts',(0.0185668417359279,1.1167273750012,0.12));
#5211=CARTESIAN_POINT('Ctrl Pts',(-0.011277474795416,1.11564956182599,0.));
#5212=CARTESIAN_POINT('Ctrl Pts',(-0.011277474795416,1.11564956182599,0.12));
#5213=CARTESIAN_POINT('Ctrl Pts',(-0.041066019590905,1.11377396404697,0.));
#5214=CARTESIAN_POINT('Ctrl Pts',(-0.041066019590905,1.11377396404697,0.12));
#5215=CARTESIAN_POINT('Ctrl Pts',(-0.0707774336926752,1.11110240713063,
0.));
#5216=CARTESIAN_POINT('Ctrl Pts',(-0.0707774336926752,1.11110240713063,
0.12));
#5217=CARTESIAN_POINT('Ctrl Pts',(-0.100390386189687,1.10763730457062,0.));
#5218=CARTESIAN_POINT('Ctrl Pts',(-0.100390386189687,1.10763730457062,0.12));
#5219=CARTESIAN_POINT('Ctrl Pts',(-0.129883601129753,1.10338164243566,0.));
#5220=CARTESIAN_POINT('Ctrl Pts',(-0.129883601129753,1.10338164243566,0.12));
#5221=CARTESIAN_POINT('Ctrl Pts',(-0.159235881741536,1.09833896639078,0.));
#5222=CARTESIAN_POINT('Ctrl Pts',(-0.159235881741536,1.09833896639078,0.12));
#5223=CARTESIAN_POINT('Ctrl Pts',(-0.188426134393585,1.09251336987768,0.));
#5224=CARTESIAN_POINT('Ctrl Pts',(-0.188426134393585,1.09251336987768,0.12));
#5225=CARTESIAN_POINT('Ctrl Pts',(-0.217433396017983,1.08590947721851,0.));
#5226=CARTESIAN_POINT('Ctrl Pts',(-0.217433396017983,1.08590947721851,0.12));
#5227=CARTESIAN_POINT('Ctrl Pts',(-0.246236848114778,1.07853244619972,0.));
#5228=CARTESIAN_POINT('Ctrl Pts',(-0.246236848114778,1.07853244619972,0.12));
#5229=CARTESIAN_POINT('Ctrl Pts',(-0.274815813222603,1.07038799540312,0.));
#5230=CARTESIAN_POINT('Ctrl Pts',(-0.274815813222603,1.07038799540312,0.12));
#5231=CARTESIAN_POINT('Ctrl Pts',(-0.303149754470475,1.06148242804708,0.));
#5232=CARTESIAN_POINT('Ctrl Pts',(-0.303149754470475,1.06148242804708,0.12));
#5233=CARTESIAN_POINT('Ctrl Pts',(-0.3312182767774,1.05182265203972,0.));
#5234=CARTESIAN_POINT('Ctrl Pts',(-0.3312182767774,1.05182265203972,0.12));
#5235=CARTESIAN_POINT('Ctrl Pts',(-0.359001120477101,1.04141621492845,0.));
#5236=CARTESIAN_POINT('Ctrl Pts',(-0.359001120477101,1.04141621492845,0.12));
#5237=CARTESIAN_POINT('Ctrl Pts',(-0.386478184359588,1.03027128325725,0.));
#5238=CARTESIAN_POINT('Ctrl Pts',(-0.386478184359588,1.03027128325725,0.12));
#5239=CARTESIAN_POINT('Ctrl Pts',(-0.413629579915113,1.01839656305955,0.));
#5240=CARTESIAN_POINT('Ctrl Pts',(-0.413629579915113,1.01839656305955,0.12));
#5241=CARTESIAN_POINT('Ctrl Pts',(-0.440435680606144,1.00580123015714,0.));
#5242=CARTESIAN_POINT('Ctrl Pts',(-0.440435680606144,1.00580123015714,0.12));
#5243=CARTESIAN_POINT('Ctrl Pts',(-0.466877166338154,0.992494869297873,
0.));
#5244=CARTESIAN_POINT('Ctrl Pts',(-0.466877166338154,0.992494869297873,
0.12));
#5245=CARTESIAN_POINT('Ctrl Pts',(-0.492935086995497,0.97848737862061,0.));
#5246=CARTESIAN_POINT('Ctrl Pts',(-0.492935086995497,0.97848737862061,0.12));
#5247=CARTESIAN_POINT('Ctrl Pts',(-0.518590849350232,0.963789014835687,
0.));
#5248=CARTESIAN_POINT('Ctrl Pts',(-0.518590849350232,0.963789014835687,
0.12));
#5249=CARTESIAN_POINT('Ctrl Pts',(-0.5438261402299,0.948410555212641,0.));
#5250=CARTESIAN_POINT('Ctrl Pts',(-0.5438261402299,0.948410555212641,0.12));
#5251=CARTESIAN_POINT('Ctrl Pts',(-0.568622860345892,0.932363440835325,
0.));
#5252=CARTESIAN_POINT('Ctrl Pts',(-0.568622860345892,0.932363440835325,
0.12));
#5253=CARTESIAN_POINT('Ctrl Pts',(-0.592963069825743,0.91565989731825,0.));
#5254=CARTESIAN_POINT('Ctrl Pts',(-0.592963069825743,0.91565989731825,0.12));
#5255=CARTESIAN_POINT('Ctrl Pts',(-0.616828889168791,0.898313140761531,
0.));
#5256=CARTESIAN_POINT('Ctrl Pts',(-0.616828889168791,0.898313140761531,
0.12));
#5257=CARTESIAN_POINT('Ctrl Pts',(-0.64020259788639,0.880337207900991,0.));
#5258=CARTESIAN_POINT('Ctrl Pts',(-0.64020259788639,0.880337207900991,0.12));
#5259=CARTESIAN_POINT('Ctrl Pts',(-0.663066855029865,0.861746554484547,
0.));
#5260=CARTESIAN_POINT('Ctrl Pts',(-0.663066855029865,0.861746554484547,
0.12));
#5261=CARTESIAN_POINT('Ctrl Pts',(-0.685404899341948,0.842555693142475,
0.));
#5262=CARTESIAN_POINT('Ctrl Pts',(-0.685404899341948,0.842555693142475,
0.12));
#5263=CARTESIAN_POINT('Ctrl Pts',(-0.707200722570447,0.822778881439102,
0.));
#5264=CARTESIAN_POINT('Ctrl Pts',(-0.707200722570447,0.822778881439102,
0.12));
#5265=CARTESIAN_POINT('Ctrl Pts',(-0.728439343632102,0.802429621210551,
0.));
#5266=CARTESIAN_POINT('Ctrl Pts',(-0.728439343632102,0.802429621210551,
0.12));
#5267=CARTESIAN_POINT('Ctrl Pts',(-0.749106566400217,0.781521126617609,
0.));
#5268=CARTESIAN_POINT('Ctrl Pts',(-0.749106566400217,0.781521126617609,
0.12));
#5269=CARTESIAN_POINT('Ctrl Pts',(-0.76918851698896,0.760067206050081,0.));
#5270=CARTESIAN_POINT('Ctrl Pts',(-0.76918851698896,0.760067206050081,0.12));
#5271=CARTESIAN_POINT('Ctrl Pts',(-0.788671222413612,0.738083066750512,
0.));
#5272=CARTESIAN_POINT('Ctrl Pts',(-0.788671222413612,0.738083066750512,
0.12));
#5273=CARTESIAN_POINT('Ctrl Pts',(-0.807540237001567,0.715586030006559,
0.));
#5274=CARTESIAN_POINT('Ctrl Pts',(-0.807540237001567,0.715586030006559,
0.12));
#5275=CARTESIAN_POINT('Ctrl Pts',(-0.825780081176955,0.692596598957924,
0.));
#5276=CARTESIAN_POINT('Ctrl Pts',(-0.825780081176955,0.692596598957924,
0.12));
#5277=CARTESIAN_POINT('Ctrl Pts',(-0.843374934437182,0.669137170123487,
0.));
#5278=CARTESIAN_POINT('Ctrl Pts',(-0.843374934437182,0.669137170123487,
0.12));
#5279=CARTESIAN_POINT('Ctrl Pts',(-0.860309667736862,0.645230105164959,
0.));
#5280=CARTESIAN_POINT('Ctrl Pts',(-0.860309667736862,0.645230105164959,
0.12));
#5281=CARTESIAN_POINT('Ctrl Pts',(-0.876570783334186,0.620895981731371,
0.));
#5282=CARTESIAN_POINT('Ctrl Pts',(-0.876570783334186,0.620895981731371,
0.12));
#5283=CARTESIAN_POINT('Ctrl Pts',(-0.892147344046454,0.596151853069194,
0.));
#5284=CARTESIAN_POINT('Ctrl Pts',(-0.892147344046454,0.596151853069194,
0.12));
#5285=CARTESIAN_POINT('Ctrl Pts',(-0.90703203930424,0.571009280629087,0.));
#5286=CARTESIAN_POINT('Ctrl Pts',(-0.90703203930424,0.571009280629087,0.12));
#5287=CARTESIAN_POINT('Ctrl Pts',(-0.921220578942929,0.545475192012713,
0.));
#5288=CARTESIAN_POINT('Ctrl Pts',(-0.921220578942929,0.545475192012713,
0.12));
#5289=CARTESIAN_POINT('Ctrl Pts',(-0.932012813071653,0.524737521565861,
0.));
#5290=CARTESIAN_POINT('Ctrl Pts',(-0.932012813071653,0.524737521565861,
0.12));
#5291=CARTESIAN_POINT('Ctrl Pts',(-0.939792491219411,0.509010207622601,
0.));
#5292=CARTESIAN_POINT('Ctrl Pts',(-0.939792491219411,0.509010207622601,
0.12));
#5293=CARTESIAN_POINT('Ctrl Pts',(-0.944839172149305,0.498447974675534,
0.));
#5294=CARTESIAN_POINT('Ctrl Pts',(-0.944839172149305,0.498447974675534,
0.12));
#5295=CARTESIAN_POINT('Ctrl Pts',(-0.94732756983434,0.493147518935017,0.));
#5296=CARTESIAN_POINT('Ctrl Pts',(-0.94732756983434,0.493147518935017,0.12));
#5297=CARTESIAN_POINT('Ctrl Pts',(-0.8680312528477,-0.633495422775274,0.12));
#5298=CARTESIAN_POINT('Ctrl Pts',(-0.866468860926997,-0.635830722731769,
0.12));
#5299=CARTESIAN_POINT('Ctrl Pts',(-0.861627881960007,-0.64301558066062,
0.12));
#5300=CARTESIAN_POINT('Ctrl Pts',(-0.853391883864834,-0.654977418032855,
0.12));
#5301=CARTESIAN_POINT('Ctrl Pts',(-0.841545334406876,-0.671576597784011,
0.12));
#5302=CARTESIAN_POINT('Ctrl Pts',(-0.82578008117756,-0.69259659895799,0.12));
#5303=CARTESIAN_POINT('Ctrl Pts',(-0.807540237001814,-0.715586030006588,
0.12));
#5304=CARTESIAN_POINT('Ctrl Pts',(-0.788671222413511,-0.738083066750504,
0.12));
#5305=CARTESIAN_POINT('Ctrl Pts',(-0.769188516988648,-0.760067206050057,
0.12));
#5306=CARTESIAN_POINT('Ctrl Pts',(-0.749106566399864,-0.781521126617586,
0.12));
#5307=CARTESIAN_POINT('Ctrl Pts',(-0.728439343631846,-0.802429621210541,
0.12));
#5308=CARTESIAN_POINT('Ctrl Pts',(-0.707200722570354,-0.822778881439107,
0.12));
#5309=CARTESIAN_POINT('Ctrl Pts',(-0.685404899341998,-0.84255569314248,
0.12));
#5310=CARTESIAN_POINT('Ctrl Pts',(-0.663066855029994,-0.861746554484541,
0.12));
#5311=CARTESIAN_POINT('Ctrl Pts',(-0.640202597886525,-0.880337207900968,
0.12));
#5312=CARTESIAN_POINT('Ctrl Pts',(-0.61682888916888,-0.898313140761512,
0.12));
#5313=CARTESIAN_POINT('Ctrl Pts',(-0.592963069825771,-0.915659897318245,
0.12));
#5314=CARTESIAN_POINT('Ctrl Pts',(-0.568622860345861,-0.932363440835334,
0.12));
#5315=CARTESIAN_POINT('Ctrl Pts',(-0.543826140229843,-0.948410555212658,
0.12));
#5316=CARTESIAN_POINT('Ctrl Pts',(-0.518590849350175,-0.963789014835703,
0.12));
#5317=CARTESIAN_POINT('Ctrl Pts',(-0.492935086995462,-0.978487378620622,
0.12));
#5318=CARTESIAN_POINT('Ctrl Pts',(-0.466877166338143,-0.992494869297879,
0.12));
#5319=CARTESIAN_POINT('Ctrl Pts',(-0.440435680606148,-1.00580123015714,
0.12));
#5320=CARTESIAN_POINT('Ctrl Pts',(-0.413629579915119,-1.01839656305955,
0.12));
#5321=CARTESIAN_POINT('Ctrl Pts',(-0.386478184359591,-1.03027128325725,
0.12));
#5322=CARTESIAN_POINT('Ctrl Pts',(-0.359001120477101,-1.04141621492846,
0.12));
#5323=CARTESIAN_POINT('Ctrl Pts',(-0.331218276777395,-1.05182265203972,
0.12));
#5324=CARTESIAN_POINT('Ctrl Pts',(-0.30314975447047,-1.06148242804708,0.12));
#5325=CARTESIAN_POINT('Ctrl Pts',(-0.2748158132226,-1.07038799540312,0.12));
#5326=CARTESIAN_POINT('Ctrl Pts',(-0.246236848114779,-1.07853244619974,
0.12));
#5327=CARTESIAN_POINT('Ctrl Pts',(-0.217433396017985,-1.08590947721852,
0.12));
#5328=CARTESIAN_POINT('Ctrl Pts',(-0.188426134393584,-1.09251336987768,
0.12));
#5329=CARTESIAN_POINT('Ctrl Pts',(-0.159235881741527,-1.09833896639077,
0.12));
#5330=CARTESIAN_POINT('Ctrl Pts',(-0.129883601129733,-1.10338164243564,
0.12));
#5331=CARTESIAN_POINT('Ctrl Pts',(-0.100390386189668,-1.1076373045706,0.12));
#5332=CARTESIAN_POINT('Ctrl Pts',(-0.0707774336926613,-1.11110240713062,
0.12));
#5333=CARTESIAN_POINT('Ctrl Pts',(-0.0410660195909007,-1.11377396404697,
0.12));
#5334=CARTESIAN_POINT('Ctrl Pts',(-0.0112774747954127,-1.11564956182599,
0.12));
#5335=CARTESIAN_POINT('Ctrl Pts',(0.0185668417359402,-1.11672737500119,
0.12));
#5336=CARTESIAN_POINT('Ctrl Pts',(0.0484455558693415,-1.11700616793207,
0.12));
#5337=CARTESIAN_POINT('Ctrl Pts',(0.0783372821756426,-1.11648528736655,
0.12));
#5338=CARTESIAN_POINT('Ctrl Pts',(0.108220629786098,-1.11516465787405,0.12));
#5339=CARTESIAN_POINT('Ctrl Pts',(0.138074209040328,-1.1130447764894,0.12));
#5340=CARTESIAN_POINT('Ctrl Pts',(0.167876633777266,-1.11012670736124,0.12));
#5341=CARTESIAN_POINT('Ctrl Pts',(0.197606544321918,-1.10641207905813,0.12));
#5342=CARTESIAN_POINT('Ctrl Pts',(0.227242642150327,-1.10190308368776,0.12));
#5343=CARTESIAN_POINT('Ctrl Pts',(0.256763722532457,-1.09660247571268,0.12));
#5344=CARTESIAN_POINT('Ctrl Pts',(0.286148704656023,-1.09051357088032,0.12));
#5345=CARTESIAN_POINT('Ctrl Pts',(0.315376671295726,-1.08364024578391,0.12));
#5346=CARTESIAN_POINT('Ctrl Pts',(0.344426864523868,-1.07598693493533,0.12));
#5347=CARTESIAN_POINT('Ctrl Pts',(0.373278657560889,-1.06755862629372,0.12));
#5348=CARTESIAN_POINT('Ctrl Pts',(0.40191153059007,-1.05836085760139,0.12));
#5349=CARTESIAN_POINT('Ctrl Pts',(0.430305052465067,-1.04839971220046,0.12));
#5350=CARTESIAN_POINT('Ctrl Pts',(0.45843884125875,-1.03768181616585,0.12));
#5351=CARTESIAN_POINT('Ctrl Pts',(0.486292621102405,-1.02621433076827,0.12));
#5352=CARTESIAN_POINT('Ctrl Pts',(0.513846332693361,-1.01400494236352,0.12));
#5353=CARTESIAN_POINT('Ctrl Pts',(0.541080235433912,-1.00106185298107,0.12));
#5354=CARTESIAN_POINT('Ctrl Pts',(0.567974995595113,-0.987393771329312,
0.12));
#5355=CARTESIAN_POINT('Ctrl Pts',(0.594511824092215,-0.973009902467593,
0.12));
#5356=CARTESIAN_POINT('Ctrl Pts',(0.620672396673315,-0.957919944163756,
0.12));
#5357=CARTESIAN_POINT('Ctrl Pts',(0.646438641619482,-0.942134087249009,
0.12));
#5358=CARTESIAN_POINT('Ctrl Pts',(0.67179254905522,-0.925663015702513,0.12));
#5359=CARTESIAN_POINT('Ctrl Pts',(0.696716011515847,-0.908517905290565,
0.12));
#5360=CARTESIAN_POINT('Ctrl Pts',(0.721190552023322,-0.890710427237186,
0.12));
#5361=CARTESIAN_POINT('Ctrl Pts',(0.745197525414791,-0.872252731655685,
0.12));
#5362=CARTESIAN_POINT('Ctrl Pts',(0.768718652031186,-0.853157416735685,
0.12));
#5363=CARTESIAN_POINT('Ctrl Pts',(0.791736496209353,-0.833437500599933,
0.12));
#5364=CARTESIAN_POINT('Ctrl Pts',(0.814234876393174,-0.81310639575503,0.12));
#5365=CARTESIAN_POINT('Ctrl Pts',(0.836199528793963,-0.792177873864096,
0.12));
#5366=CARTESIAN_POINT('Ctrl Pts',(0.857617760934752,-0.770666069833932,
0.12));
#5367=CARTESIAN_POINT('Ctrl Pts',(0.878477242115376,-0.74858551944097,0.12));
#5368=CARTESIAN_POINT('Ctrl Pts',(0.898764943113291,-0.725951191437368,
0.12));
#5369=CARTESIAN_POINT('Ctrl Pts',(0.918466214618678,-0.70277851394702,0.12));
#5370=CARTESIAN_POINT('Ctrl Pts',(0.937563319582499,-0.679083423181946,
0.12));
#5371=CARTESIAN_POINT('Ctrl Pts',(0.956036026761672,-0.654882328595489,
0.12));
#5372=CARTESIAN_POINT('Ctrl Pts',(0.973864462863685,-0.630191986422907,
0.12));
#5373=CARTESIAN_POINT('Ctrl Pts',(0.991031566790864,-0.605029389584474,
0.12));
#5374=CARTESIAN_POINT('Ctrl Pts',(1.00752529081786,-0.579411667627393,0.12));
#5375=CARTESIAN_POINT('Ctrl Pts',(1.02334191285221,-0.553355942423953,0.12));
#5376=CARTESIAN_POINT('Ctrl Pts',(1.03848536635828,-0.526879343018338,0.12));
#5377=CARTESIAN_POINT('Ctrl Pts',(1.05296063073153,-0.499999257829972,0.12));
#5378=CARTESIAN_POINT('Ctrl Pts',(1.06676816041365,-0.472733545459157,0.12));
#5379=CARTESIAN_POINT('Ctrl Pts',(1.0798986829592,-0.44510073074649,0.12));
#5380=CARTESIAN_POINT('Ctrl Pts',(1.09232595504273,-0.417120282666841,0.12));
#5381=CARTESIAN_POINT('Ctrl Pts',(1.1040065500515,-0.388812610728411,0.12));
#5382=CARTESIAN_POINT('Ctrl Pts',(1.11489509573247,-0.360198442057814,0.12));
#5383=CARTESIAN_POINT('Ctrl Pts',(1.12495696400084,-0.331298301519,0.12));
#5384=CARTESIAN_POINT('Ctrl Pts',(1.13418071785862,-0.302131999517994,0.12));
#5385=CARTESIAN_POINT('Ctrl Pts',(1.14259364432097,-0.272718001214759,0.12));
#5386=CARTESIAN_POINT('Ctrl Pts',(1.15026681194464,-0.243073201156197,0.12));
#5387=CARTESIAN_POINT('Ctrl Pts',(1.15728135528338,-0.213214209193066,0.12));
#5388=CARTESIAN_POINT('Ctrl Pts',(1.16370031035361,-0.183158411923726,0.12));
#5389=CARTESIAN_POINT('Ctrl Pts',(1.1695394362355,-0.152925093725504,0.12));
#5390=CARTESIAN_POINT('Ctrl Pts',(1.17473573615846,-0.1225365994934,0.12));
#5391=CARTESIAN_POINT('Ctrl Pts',(1.17912488557723,-0.0920192855934153,
0.12));
#5392=CARTESIAN_POINT('Ctrl Pts',(1.18249458653374,-0.0614026081204919,
0.12));
#5393=CARTESIAN_POINT('Ctrl Pts',(1.18463081328693,-0.0307183863950716,
0.12));
#5394=CARTESIAN_POINT('Ctrl Pts',(1.18536679600018,3.34053531364509E-15,
0.12));
#5395=CARTESIAN_POINT('Ctrl Pts',(1.18463081328694,0.0307183863950759,0.12));
#5396=CARTESIAN_POINT('Ctrl Pts',(1.18249458653375,0.0614026081204918,0.12));
#5397=CARTESIAN_POINT('Ctrl Pts',(1.17912488557725,0.0920192855934129,0.12));
#5398=CARTESIAN_POINT('Ctrl Pts',(1.17473573615847,0.122536599493401,0.12));
#5399=CARTESIAN_POINT('Ctrl Pts',(1.1695394362355,0.152925093725509,0.12));
#5400=CARTESIAN_POINT('Ctrl Pts',(1.1637003103536,0.183158411923732,0.12));
#5401=CARTESIAN_POINT('Ctrl Pts',(1.15728135528336,0.21321420919307,0.12));
#5402=CARTESIAN_POINT('Ctrl Pts',(1.15026681194462,0.243073201156195,0.12));
#5403=CARTESIAN_POINT('Ctrl Pts',(1.14259364432096,0.272718001214758,0.12));
#5404=CARTESIAN_POINT('Ctrl Pts',(1.13418071785862,0.302131999517997,0.12));
#5405=CARTESIAN_POINT('Ctrl Pts',(1.12495696400085,0.33129830151901,0.12));
#5406=CARTESIAN_POINT('Ctrl Pts',(1.11489509573248,0.36019844205783,0.12));
#5407=CARTESIAN_POINT('Ctrl Pts',(1.10400655005151,0.388812610728428,0.12));
#5408=CARTESIAN_POINT('Ctrl Pts',(1.09232595504274,0.417120282666858,0.12));
#5409=CARTESIAN_POINT('Ctrl Pts',(1.0798986829592,0.4451007307465,0.12));
#5410=CARTESIAN_POINT('Ctrl Pts',(1.06676816041364,0.472733545459153,0.12));
#5411=CARTESIAN_POINT('Ctrl Pts',(1.05296063073151,0.499999257829953,0.12));
#5412=CARTESIAN_POINT('Ctrl Pts',(1.03848536635825,0.526879343018311,0.12));
#5413=CARTESIAN_POINT('Ctrl Pts',(1.02334191285218,0.553355942423933,0.12));
#5414=CARTESIAN_POINT('Ctrl Pts',(1.00752529081784,0.579411667627389,0.12));
#5415=CARTESIAN_POINT('Ctrl Pts',(0.991031566790874,0.605029389584491,0.12));
#5416=CARTESIAN_POINT('Ctrl Pts',(0.973864462863717,0.630191986422942,0.12));
#5417=CARTESIAN_POINT('Ctrl Pts',(0.956036026761713,0.654882328595531,0.12));
#5418=CARTESIAN_POINT('Ctrl Pts',(0.93756331958253,0.67908342318198,0.12));
#5419=CARTESIAN_POINT('Ctrl Pts',(0.918466214618686,0.702778513947035,0.12));
#5420=CARTESIAN_POINT('Ctrl Pts',(0.898764943113273,0.725951191437361,0.12));
#5421=CARTESIAN_POINT('Ctrl Pts',(0.87847724211534,0.748585519440939,0.12));
#5422=CARTESIAN_POINT('Ctrl Pts',(0.857617760934708,0.770666069833888,0.12));
#5423=CARTESIAN_POINT('Ctrl Pts',(0.836199528793927,0.792177873864058,0.12));
#5424=CARTESIAN_POINT('Ctrl Pts',(0.814234876393157,0.813106395755015,0.12));
#5425=CARTESIAN_POINT('Ctrl Pts',(0.79173649620936,0.833437500599952,0.12));
#5426=CARTESIAN_POINT('Ctrl Pts',(0.768718652031217,0.853157416735736,0.12));
#5427=CARTESIAN_POINT('Ctrl Pts',(0.745197525414833,0.872252731655753,0.12));
#5428=CARTESIAN_POINT('Ctrl Pts',(0.721190552023354,0.890710427237242,0.12));
#5429=CARTESIAN_POINT('Ctrl Pts',(0.696716011515856,0.908517905290589,0.12));
#5430=CARTESIAN_POINT('Ctrl Pts',(0.671792549055205,0.9256630157025,0.12));
#5431=CARTESIAN_POINT('Ctrl Pts',(0.64643864161945,0.942134087248967,0.12));
#5432=CARTESIAN_POINT('Ctrl Pts',(0.620672396673277,0.95791994416371,0.12));
#5433=CARTESIAN_POINT('Ctrl Pts',(0.594511824092183,0.973009902467561,0.12));
#5434=CARTESIAN_POINT('Ctrl Pts',(0.567974995595098,0.987393771329304,0.12));
#5435=CARTESIAN_POINT('Ctrl Pts',(0.541080235433915,1.00106185298108,0.12));
#5436=CARTESIAN_POINT('Ctrl Pts',(0.513846332693379,1.01400494236354,0.12));
#5437=CARTESIAN_POINT('Ctrl Pts',(0.486292621102429,1.02621433076829,0.12));
#5438=CARTESIAN_POINT('Ctrl Pts',(0.458438841258773,1.03768181616586,0.12));
#5439=CARTESIAN_POINT('Ctrl Pts',(0.430305052465076,1.04839971220046,0.12));
#5440=CARTESIAN_POINT('Ctrl Pts',(0.401911530590058,1.05836085760139,0.12));
#5441=CARTESIAN_POINT('Ctrl Pts',(0.373278657560858,1.06755862629372,0.12));
#5442=CARTESIAN_POINT('Ctrl Pts',(0.344426864523825,1.07598693493533,0.12));
#5443=CARTESIAN_POINT('Ctrl Pts',(0.315376671295687,1.08364024578392,0.12));
#5444=CARTESIAN_POINT('Ctrl Pts',(0.286148704656,1.09051357088032,0.12));
#5445=CARTESIAN_POINT('Ctrl Pts',(0.256763722532462,1.09660247571268,0.12));
#5446=CARTESIAN_POINT('Ctrl Pts',(0.22724264215036,1.10190308368774,0.12));
#5447=CARTESIAN_POINT('Ctrl Pts',(0.197606544321966,1.10641207905811,0.12));
#5448=CARTESIAN_POINT('Ctrl Pts',(0.167876633777302,1.11012670736122,0.12));
#5449=CARTESIAN_POINT('Ctrl Pts',(0.138074209040338,1.11304477648939,0.12));
#5450=CARTESIAN_POINT('Ctrl Pts',(0.108220629786082,1.11516465787406,0.12));
#5451=CARTESIAN_POINT('Ctrl Pts',(0.0783372821756164,1.11648528736656,0.12));
#5452=CARTESIAN_POINT('Ctrl Pts',(0.0484455558693182,1.11700616793208,0.12));
#5453=CARTESIAN_POINT('Ctrl Pts',(0.0185668417359279,1.1167273750012,0.12));
#5454=CARTESIAN_POINT('Ctrl Pts',(-0.011277474795416,1.11564956182599,0.12));
#5455=CARTESIAN_POINT('Ctrl Pts',(-0.041066019590905,1.11377396404697,0.12));
#5456=CARTESIAN_POINT('Ctrl Pts',(-0.0707774336926752,1.11110240713063,
0.12));
#5457=CARTESIAN_POINT('Ctrl Pts',(-0.100390386189687,1.10763730457062,0.12));
#5458=CARTESIAN_POINT('Ctrl Pts',(-0.129883601129753,1.10338164243566,0.12));
#5459=CARTESIAN_POINT('Ctrl Pts',(-0.159235881741536,1.09833896639078,0.12));
#5460=CARTESIAN_POINT('Ctrl Pts',(-0.188426134393585,1.09251336987768,0.12));
#5461=CARTESIAN_POINT('Ctrl Pts',(-0.217433396017983,1.08590947721851,0.12));
#5462=CARTESIAN_POINT('Ctrl Pts',(-0.246236848114778,1.07853244619972,0.12));
#5463=CARTESIAN_POINT('Ctrl Pts',(-0.274815813222603,1.07038799540312,0.12));
#5464=CARTESIAN_POINT('Ctrl Pts',(-0.303149754470475,1.06148242804708,0.12));
#5465=CARTESIAN_POINT('Ctrl Pts',(-0.3312182767774,1.05182265203972,0.12));
#5466=CARTESIAN_POINT('Ctrl Pts',(-0.359001120477101,1.04141621492845,0.12));
#5467=CARTESIAN_POINT('Ctrl Pts',(-0.386478184359588,1.03027128325725,0.12));
#5468=CARTESIAN_POINT('Ctrl Pts',(-0.413629579915113,1.01839656305955,0.12));
#5469=CARTESIAN_POINT('Ctrl Pts',(-0.440435680606144,1.00580123015714,0.12));
#5470=CARTESIAN_POINT('Ctrl Pts',(-0.466877166338154,0.992494869297873,
0.12));
#5471=CARTESIAN_POINT('Ctrl Pts',(-0.492935086995497,0.97848737862061,0.12));
#5472=CARTESIAN_POINT('Ctrl Pts',(-0.518590849350232,0.963789014835687,
0.12));
#5473=CARTESIAN_POINT('Ctrl Pts',(-0.5438261402299,0.948410555212641,0.12));
#5474=CARTESIAN_POINT('Ctrl Pts',(-0.568622860345892,0.932363440835325,
0.12));
#5475=CARTESIAN_POINT('Ctrl Pts',(-0.592963069825743,0.91565989731825,0.12));
#5476=CARTESIAN_POINT('Ctrl Pts',(-0.616828889168791,0.898313140761531,
0.12));
#5477=CARTESIAN_POINT('Ctrl Pts',(-0.64020259788639,0.880337207900991,0.12));
#5478=CARTESIAN_POINT('Ctrl Pts',(-0.663066855029865,0.861746554484547,
0.12));
#5479=CARTESIAN_POINT('Ctrl Pts',(-0.685404899341948,0.842555693142475,
0.12));
#5480=CARTESIAN_POINT('Ctrl Pts',(-0.707200722570447,0.822778881439102,
0.12));
#5481=CARTESIAN_POINT('Ctrl Pts',(-0.728439343632102,0.802429621210551,
0.12));
#5482=CARTESIAN_POINT('Ctrl Pts',(-0.749106566400217,0.781521126617609,
0.12));
#5483=CARTESIAN_POINT('Ctrl Pts',(-0.76918851698896,0.760067206050081,0.12));
#5484=CARTESIAN_POINT('Ctrl Pts',(-0.788671222413612,0.738083066750512,
0.12));
#5485=CARTESIAN_POINT('Ctrl Pts',(-0.807540237001567,0.715586030006559,
0.12));
#5486=CARTESIAN_POINT('Ctrl Pts',(-0.825780081176955,0.692596598957924,
0.12));
#5487=CARTESIAN_POINT('Ctrl Pts',(-0.841545334406124,0.671576597783911,
0.12));
#5488=CARTESIAN_POINT('Ctrl Pts',(-0.85339188386416,0.654977418032737,0.12));
#5489=CARTESIAN_POINT('Ctrl Pts',(-0.861627881959507,0.643015580660492,
0.12));
#5490=CARTESIAN_POINT('Ctrl Pts',(-0.866468860926645,0.635830722731627,
0.12));
#5491=CARTESIAN_POINT('Ctrl Pts',(-0.868031252847412,0.633495422775111,
0.12));
#5492=CARTESIAN_POINT('Origin',(0.11901961308292,6.21724893790088E-15,0.12));
#5493=CARTESIAN_POINT('',(0.,0.,0.));
#5494=CARTESIAN_POINT('',(0.,0.,0.));
#5495=CARTESIAN_POINT('',(0.,6.52,4.5));
#5496=CARTESIAN_POINT('',(0.,0.,0.));
#5497=CARTESIAN_POINT('',(0.,0.,0.));
#5498=UNCERTAINTY_MEASURE_WITH_UNIT(LENGTH_MEASURE(0.001),#5536,
'DISTANCE_ACCURACY_VALUE',
'Maximum model space distance between geometric entities at asserted c
onnectivities');
#5499=UNCERTAINTY_MEASURE_WITH_UNIT(LENGTH_MEASURE(0.001),#5536,
'DISTANCE_ACCURACY_VALUE',
'Maximum model space distance between geometric entities at asserted c
onnectivities');
#5500=UNCERTAINTY_MEASURE_WITH_UNIT(LENGTH_MEASURE(0.001),#5536,
'DISTANCE_ACCURACY_VALUE',
'Maximum model space distance between geometric entities at asserted c
onnectivities');
#5501=UNCERTAINTY_MEASURE_WITH_UNIT(LENGTH_MEASURE(0.001),#5536,
'DISTANCE_ACCURACY_VALUE',
'Maximum model space distance between geometric entities at asserted c
onnectivities');
#5502=UNCERTAINTY_MEASURE_WITH_UNIT(LENGTH_MEASURE(0.001),#5536,
'DISTANCE_ACCURACY_VALUE',
'Maximum model space distance between geometric entities at asserted c
onnectivities');
#5503=UNCERTAINTY_MEASURE_WITH_UNIT(LENGTH_MEASURE(0.001),#5536,
'DISTANCE_ACCURACY_VALUE',
'Maximum model space distance between geometric entities at asserted c
onnectivities');
#5504=UNCERTAINTY_MEASURE_WITH_UNIT(LENGTH_MEASURE(0.001),#5536,
'DISTANCE_ACCURACY_VALUE',
'Maximum model space distance between geometric entities at asserted c
onnectivities');
#5505=UNCERTAINTY_MEASURE_WITH_UNIT(LENGTH_MEASURE(0.001),#5536,
'DISTANCE_ACCURACY_VALUE',
'Maximum model space distance between geometric entities at asserted c
onnectivities');
#5506=UNCERTAINTY_MEASURE_WITH_UNIT(LENGTH_MEASURE(0.001),#5536,
'DISTANCE_ACCURACY_VALUE',
'Maximum model space distance between geometric entities at asserted c
onnectivities');
#5507=UNCERTAINTY_MEASURE_WITH_UNIT(LENGTH_MEASURE(0.001),#5536,
'DISTANCE_ACCURACY_VALUE',
'Maximum model space distance between geometric entities at asserted c
onnectivities');
#5508=UNCERTAINTY_MEASURE_WITH_UNIT(LENGTH_MEASURE(0.001),#5536,
'DISTANCE_ACCURACY_VALUE',
'Maximum model space distance between geometric entities at asserted c
onnectivities');
#5509=UNCERTAINTY_MEASURE_WITH_UNIT(LENGTH_MEASURE(0.001),#5536,
'DISTANCE_ACCURACY_VALUE',
'Maximum model space distance between geometric entities at asserted c
onnectivities');
#5510=UNCERTAINTY_MEASURE_WITH_UNIT(LENGTH_MEASURE(0.001),#5536,
'DISTANCE_ACCURACY_VALUE',
'Maximum model space distance between geometric entities at asserted c
onnectivities');
#5511=UNCERTAINTY_MEASURE_WITH_UNIT(LENGTH_MEASURE(0.001),#5536,
'DISTANCE_ACCURACY_VALUE',
'Maximum model space distance between geometric entities at asserted c
onnectivities');
#5512=UNCERTAINTY_MEASURE_WITH_UNIT(LENGTH_MEASURE(0.001),#5536,
'DISTANCE_ACCURACY_VALUE',
'Maximum model space distance between geometric entities at asserted c
onnectivities');
#5513=UNCERTAINTY_MEASURE_WITH_UNIT(LENGTH_MEASURE(0.001),#5536,
'DISTANCE_ACCURACY_VALUE',
'Maximum model space distance between geometric entities at asserted c
onnectivities');
#5514=UNCERTAINTY_MEASURE_WITH_UNIT(LENGTH_MEASURE(0.001),#5536,
'DISTANCE_ACCURACY_VALUE',
'Maximum model space distance between geometric entities at asserted c
onnectivities');
#5515=UNCERTAINTY_MEASURE_WITH_UNIT(LENGTH_MEASURE(0.001),#5536,
'DISTANCE_ACCURACY_VALUE',
'Maximum model space distance between geometric entities at asserted c
onnectivities');
#5516=UNCERTAINTY_MEASURE_WITH_UNIT(LENGTH_MEASURE(0.001),#5536,
'DISTANCE_ACCURACY_VALUE',
'Maximum model space distance between geometric entities at asserted c
onnectivities');
#5517=(
GEOMETRIC_REPRESENTATION_CONTEXT(3)
GLOBAL_UNCERTAINTY_ASSIGNED_CONTEXT((#5498))
GLOBAL_UNIT_ASSIGNED_CONTEXT((#5536,#5538,#5539))
REPRESENTATION_CONTEXT('','3D')
);
#5518=(
GEOMETRIC_REPRESENTATION_CONTEXT(3)
GLOBAL_UNCERTAINTY_ASSIGNED_CONTEXT((#5499))
GLOBAL_UNIT_ASSIGNED_CONTEXT((#5536,#5538,#5539))
REPRESENTATION_CONTEXT('','3D')
);
#5519=(
GEOMETRIC_REPRESENTATION_CONTEXT(3)
GLOBAL_UNCERTAINTY_ASSIGNED_CONTEXT((#5500))
GLOBAL_UNIT_ASSIGNED_CONTEXT((#5536,#5538,#5539))
REPRESENTATION_CONTEXT('','3D')
);
#5520=(
GEOMETRIC_REPRESENTATION_CONTEXT(3)
GLOBAL_UNCERTAINTY_ASSIGNED_CONTEXT((#5501))
GLOBAL_UNIT_ASSIGNED_CONTEXT((#5536,#5538,#5539))
REPRESENTATION_CONTEXT('','3D')
);
#5521=(
GEOMETRIC_REPRESENTATION_CONTEXT(3)
GLOBAL_UNCERTAINTY_ASSIGNED_CONTEXT((#5502))
GLOBAL_UNIT_ASSIGNED_CONTEXT((#5536,#5538,#5539))
REPRESENTATION_CONTEXT('','3D')
);
#5522=(
GEOMETRIC_REPRESENTATION_CONTEXT(3)
GLOBAL_UNCERTAINTY_ASSIGNED_CONTEXT((#5503))
GLOBAL_UNIT_ASSIGNED_CONTEXT((#5536,#5538,#5539))
REPRESENTATION_CONTEXT('','3D')
);
#5523=(
GEOMETRIC_REPRESENTATION_CONTEXT(3)
GLOBAL_UNCERTAINTY_ASSIGNED_CONTEXT((#5504))
GLOBAL_UNIT_ASSIGNED_CONTEXT((#5536,#5538,#5539))
REPRESENTATION_CONTEXT('','3D')
);
#5524=(
GEOMETRIC_REPRESENTATION_CONTEXT(3)
GLOBAL_UNCERTAINTY_ASSIGNED_CONTEXT((#5505))
GLOBAL_UNIT_ASSIGNED_CONTEXT((#5536,#5538,#5539))
REPRESENTATION_CONTEXT('','3D')
);
#5525=(
GEOMETRIC_REPRESENTATION_CONTEXT(3)
GLOBAL_UNCERTAINTY_ASSIGNED_CONTEXT((#5506))
GLOBAL_UNIT_ASSIGNED_CONTEXT((#5536,#5538,#5539))
REPRESENTATION_CONTEXT('','3D')
);
#5526=(
GEOMETRIC_REPRESENTATION_CONTEXT(3)
GLOBAL_UNCERTAINTY_ASSIGNED_CONTEXT((#5507))
GLOBAL_UNIT_ASSIGNED_CONTEXT((#5536,#5538,#5539))
REPRESENTATION_CONTEXT('','3D')
);
#5527=(
GEOMETRIC_REPRESENTATION_CONTEXT(3)
GLOBAL_UNCERTAINTY_ASSIGNED_CONTEXT((#5508))
GLOBAL_UNIT_ASSIGNED_CONTEXT((#5536,#5538,#5539))
REPRESENTATION_CONTEXT('','3D')
);
#5528=(
GEOMETRIC_REPRESENTATION_CONTEXT(3)
GLOBAL_UNCERTAINTY_ASSIGNED_CONTEXT((#5509))
GLOBAL_UNIT_ASSIGNED_CONTEXT((#5536,#5538,#5539))
REPRESENTATION_CONTEXT('','3D')
);
#5529=(
GEOMETRIC_REPRESENTATION_CONTEXT(3)
GLOBAL_UNCERTAINTY_ASSIGNED_CONTEXT((#5510))
GLOBAL_UNIT_ASSIGNED_CONTEXT((#5536,#5538,#5539))
REPRESENTATION_CONTEXT('','3D')
);
#5530=(
GEOMETRIC_REPRESENTATION_CONTEXT(3)
GLOBAL_UNCERTAINTY_ASSIGNED_CONTEXT((#5511))
GLOBAL_UNIT_ASSIGNED_CONTEXT((#5536,#5538,#5539))
REPRESENTATION_CONTEXT('','3D')
);
#5531=(
GEOMETRIC_REPRESENTATION_CONTEXT(3)
GLOBAL_UNCERTAINTY_ASSIGNED_CONTEXT((#5512))
GLOBAL_UNIT_ASSIGNED_CONTEXT((#5536,#5538,#5539))
REPRESENTATION_CONTEXT('','3D')
);
#5532=(
GEOMETRIC_REPRESENTATION_CONTEXT(3)
GLOBAL_UNCERTAINTY_ASSIGNED_CONTEXT((#5513))
GLOBAL_UNIT_ASSIGNED_CONTEXT((#5536,#5538,#5539))
REPRESENTATION_CONTEXT('','3D')
);
#5533=(
GEOMETRIC_REPRESENTATION_CONTEXT(3)
GLOBAL_UNCERTAINTY_ASSIGNED_CONTEXT((#5514))
GLOBAL_UNIT_ASSIGNED_CONTEXT((#5536,#5538,#5539))
REPRESENTATION_CONTEXT('','3D')
);
#5534=(
GEOMETRIC_REPRESENTATION_CONTEXT(3)
GLOBAL_UNCERTAINTY_ASSIGNED_CONTEXT((#5515))
GLOBAL_UNIT_ASSIGNED_CONTEXT((#5536,#5538,#5539))
REPRESENTATION_CONTEXT('','3D')
);
#5535=(
GEOMETRIC_REPRESENTATION_CONTEXT(3)
GLOBAL_UNCERTAINTY_ASSIGNED_CONTEXT((#5516))
GLOBAL_UNIT_ASSIGNED_CONTEXT((#5536,#5538,#5539))
REPRESENTATION_CONTEXT('','3D')
);
#5536=(
LENGTH_UNIT()
NAMED_UNIT(*)
SI_UNIT(.CENTI.,.METRE.)
);
#5537=(
LENGTH_UNIT()
NAMED_UNIT(*)
SI_UNIT($,.METRE.)
);
#5538=(
NAMED_UNIT(*)
PLANE_ANGLE_UNIT()
SI_UNIT($,.RADIAN.)
);
#5539=(
NAMED_UNIT(*)
SI_UNIT($,.STERADIAN.)
SOLID_ANGLE_UNIT()
);
#5540=SHAPE_DEFINITION_REPRESENTATION(#5558,#5601);
#5541=SHAPE_DEFINITION_REPRESENTATION(#5559,#5602);
#5542=SHAPE_DEFINITION_REPRESENTATION(#5560,#5603);
#5543=SHAPE_DEFINITION_REPRESENTATION(#5561,#5604);
#5544=SHAPE_DEFINITION_REPRESENTATION(#5562,#5605);
#5545=SHAPE_DEFINITION_REPRESENTATION(#5563,#5606);
#5546=SHAPE_DEFINITION_REPRESENTATION(#5564,#5607);
#5547=SHAPE_DEFINITION_REPRESENTATION(#5565,#5608);
#5548=SHAPE_DEFINITION_REPRESENTATION(#5566,#5609);
#5549=SHAPE_DEFINITION_REPRESENTATION(#5572,#5610);
#5550=SHAPE_DEFINITION_REPRESENTATION(#5573,#5611);
#5551=SHAPE_DEFINITION_REPRESENTATION(#5574,#5612);
#5552=SHAPE_DEFINITION_REPRESENTATION(#5575,#5613);
#5553=SHAPE_DEFINITION_REPRESENTATION(#5576,#5614);
#5554=SHAPE_DEFINITION_REPRESENTATION(#5592,#5615);
#5555=SHAPE_DEFINITION_REPRESENTATION(#5593,#5616);
#5556=SHAPE_DEFINITION_REPRESENTATION(#5594,#5617);
#5557=SHAPE_DEFINITION_REPRESENTATION(#5595,#5618);
#5558=PRODUCT_DEFINITION_SHAPE('',$,#5620);
#5559=PRODUCT_DEFINITION_SHAPE('',$,#5621);
#5560=PRODUCT_DEFINITION_SHAPE('',$,#5622);
#5561=PRODUCT_DEFINITION_SHAPE('',$,#5623);
#5562=PRODUCT_DEFINITION_SHAPE('',$,#5624);
#5563=PRODUCT_DEFINITION_SHAPE('',$,#5625);
#5564=PRODUCT_DEFINITION_SHAPE('',$,#5626);
#5565=PRODUCT_DEFINITION_SHAPE('',$,#5627);
#5566=PRODUCT_DEFINITION_SHAPE('',$,#5628);
#5567=PRODUCT_DEFINITION_SHAPE($,$,#91);
#5568=PRODUCT_DEFINITION_SHAPE($,$,#92);
#5569=PRODUCT_DEFINITION_SHAPE($,$,#93);
#5570=PRODUCT_DEFINITION_SHAPE($,$,#94);
#5571=PRODUCT_DEFINITION_SHAPE($,$,#95);
#5572=PRODUCT_DEFINITION_SHAPE('',$,#5629);
#5573=PRODUCT_DEFINITION_SHAPE('',$,#5630);
#5574=PRODUCT_DEFINITION_SHAPE('',$,#5631);
#5575=PRODUCT_DEFINITION_SHAPE('',$,#5632);
#5576=PRODUCT_DEFINITION_SHAPE('',$,#5633);
#5577=PRODUCT_DEFINITION_SHAPE($,$,#96);
#5578=PRODUCT_DEFINITION_SHAPE($,$,#97);
#5579=PRODUCT_DEFINITION_SHAPE($,$,#98);
#5580=PRODUCT_DEFINITION_SHAPE($,$,#99);
#5581=PRODUCT_DEFINITION_SHAPE($,$,#100);
#5582=PRODUCT_DEFINITION_SHAPE($,$,#101);
#5583=PRODUCT_DEFINITION_SHAPE($,$,#102);
#5584=PRODUCT_DEFINITION_SHAPE($,$,#103);
#5585=PRODUCT_DEFINITION_SHAPE($,$,#104);
#5586=PRODUCT_DEFINITION_SHAPE($,$,#105);
#5587=PRODUCT_DEFINITION_SHAPE($,$,#106);
#5588=PRODUCT_DEFINITION_SHAPE($,$,#107);
#5589=PRODUCT_DEFINITION_SHAPE($,$,#108);
#5590=PRODUCT_DEFINITION_SHAPE($,$,#109);
#5591=PRODUCT_DEFINITION_SHAPE($,$,#110);
#5592=PRODUCT_DEFINITION_SHAPE('',$,#5634);
#5593=PRODUCT_DEFINITION_SHAPE('',$,#5635);
#5594=PRODUCT_DEFINITION_SHAPE('',$,#5636);
#5595=PRODUCT_DEFINITION_SHAPE('',$,#5637);
#5596=PRODUCT_DEFINITION_SHAPE($,$,#111);
#5597=PRODUCT_DEFINITION_SHAPE($,$,#112);
#5598=PRODUCT_DEFINITION_SHAPE($,$,#113);
#5599=PRODUCT_DEFINITION_SHAPE($,$,#114);
#5600=PRODUCT_DEFINITION_SHAPE($,$,#115);
#5601=SHAPE_REPRESENTATION('',(#2502,#2865,#2866),#5517);
#5602=SHAPE_REPRESENTATION('',(#2503,#2797,#2798,#2799,#2800,#2801,#2802,
#2803,#2804,#2805,#2806,#2807,#2808,#2809,#2810,#2811),#5518);
#5603=SHAPE_REPRESENTATION('',(#2504),#5519);
#5604=SHAPE_REPRESENTATION('',(#2565,#2694,#2695,#2696,#2697,#2698),#5520);
#5605=SHAPE_REPRESENTATION('',(#2566),#5521);
#5606=SHAPE_REPRESENTATION('',(#2586),#5522);
#5607=SHAPE_REPRESENTATION('',(#2606),#5523);
#5608=SHAPE_REPRESENTATION('',(#2623),#5524);
#5609=SHAPE_REPRESENTATION('',(#2677),#5525);
#5610=SHAPE_REPRESENTATION('',(#2699),#5526);
#5611=SHAPE_REPRESENTATION('',(#2708),#5527);
#5612=SHAPE_REPRESENTATION('',(#2737),#5528);
#5613=SHAPE_REPRESENTATION('',(#2746),#5529);
#5614=SHAPE_REPRESENTATION('',(#2771),#5530);
#5615=SHAPE_REPRESENTATION('',(#2812,#2862,#2863,#2864),#5531);
#5616=SHAPE_REPRESENTATION('',(#2813),#5532);
#5617=SHAPE_REPRESENTATION('',(#2835),#5533);
#5618=SHAPE_REPRESENTATION('',(#2844),#5534);
#5619=PRODUCT_DEFINITION_CONTEXT('part definition',#5675,'design');
#5620=PRODUCT_DEFINITION('PAT-030','PAT-030',
#5638,#5619);
#5621=PRODUCT_DEFINITION('Flanged housing bearings and seal caps',
'Flanged housing bearings and seal caps',#5639,#5619);
#5622=PRODUCT_DEFINITION('Flanged housing','Flanged housing',#5640,#5619);
#5623=PRODUCT_DEFINITION('Sealed Ball Bearing - 20 x 47 x 14 mm',
'Sealed Ball Bearing - 20 x 47 x 14 mm',#5641,#5619);
#5624=PRODUCT_DEFINITION('Inner ring','Inner ring',#5642,#5619);
#5625=PRODUCT_DEFINITION('Outer ring','Outer ring',#5643,#5619);
#5626=PRODUCT_DEFINITION('Balls','Balls',#5644,#5619);
#5627=PRODUCT_DEFINITION('Cage','Cage',#5645,#5619);
#5628=PRODUCT_DEFINITION('Seals 2RS','Seals 2RS',#5646,#5619);
#5629=PRODUCT_DEFINITION('Outer race spacer','Outer race spacer',#5647,
#5619);
#5630=PRODUCT_DEFINITION('Seal cap','Seal cap',#5648,#5619);
#5631=PRODUCT_DEFINITION('Dust seal envelope','Dust seal envelope',#5649,
#5619);
#5632=PRODUCT_DEFINITION('Rear cap','Rear cap',#5650,#5619);
#5633=PRODUCT_DEFINITION('Cap Screw - M4x16','Cap Screw - M4x16',#5651,
#5619);
#5634=PRODUCT_DEFINITION('Shaft spacer and retaining ring',
'Shaft spacer and retaining ring',#5652,#5619);
#5635=PRODUCT_DEFINITION('Retained shaft','Retained shaft',#5653,#5619);
#5636=PRODUCT_DEFINITION('Inner race spacer','Inner race spacer',#5654,
#5619);
#5637=PRODUCT_DEFINITION('Installed retaining ring',
'Installed retaining ring',#5655,#5619);
#5638=PRODUCT_DEFINITION_FORMATION('',$,#5677);
#5639=PRODUCT_DEFINITION_FORMATION('',$,#5678);
#5640=PRODUCT_DEFINITION_FORMATION('',$,#5679);
#5641=PRODUCT_DEFINITION_FORMATION('',$,#5680);
#5642=PRODUCT_DEFINITION_FORMATION('',$,#5681);
#5643=PRODUCT_DEFINITION_FORMATION('',$,#5682);
#5644=PRODUCT_DEFINITION_FORMATION('',$,#5683);
#5645=PRODUCT_DEFINITION_FORMATION('',$,#5684);
#5646=PRODUCT_DEFINITION_FORMATION('',$,#5685);
#5647=PRODUCT_DEFINITION_FORMATION('',$,#5686);
#5648=PRODUCT_DEFINITION_FORMATION('',$,#5687);
#5649=PRODUCT_DEFINITION_FORMATION('',$,#5688);
#5650=PRODUCT_DEFINITION_FORMATION('',$,#5689);
#5651=PRODUCT_DEFINITION_FORMATION('',$,#5690);
#5652=PRODUCT_DEFINITION_FORMATION('',$,#5691);
#5653=PRODUCT_DEFINITION_FORMATION('',$,#5692);
#5654=PRODUCT_DEFINITION_FORMATION('',$,#5693);
#5655=PRODUCT_DEFINITION_FORMATION('',$,#5694);
#5656=PRODUCT_RELATED_PRODUCT_CATEGORY('PAT-030','PAT-030',(#5677));
#5657=PRODUCT_RELATED_PRODUCT_CATEGORY(
'Flanged housing bearings and seal caps',
'Flanged housing bearings and seal caps',(#5678));
#5658=PRODUCT_RELATED_PRODUCT_CATEGORY('Flanged housing',
'Flanged housing',(#5679));
#5659=PRODUCT_RELATED_PRODUCT_CATEGORY(
'Sealed Ball Bearing - 20 x 47 x 14 mm',
'Sealed Ball Bearing - 20 x 47 x 14 mm',(#5680));
#5660=PRODUCT_RELATED_PRODUCT_CATEGORY('Inner ring','Inner ring',(#5681));
#5661=PRODUCT_RELATED_PRODUCT_CATEGORY('Outer ring','Outer ring',(#5682));
#5662=PRODUCT_RELATED_PRODUCT_CATEGORY('Balls','Balls',(#5683));
#5663=PRODUCT_RELATED_PRODUCT_CATEGORY('Cage','Cage',(#5684));
#5664=PRODUCT_RELATED_PRODUCT_CATEGORY('Seals 2RS','Seals 2RS',(#5685));
#5665=PRODUCT_RELATED_PRODUCT_CATEGORY('Outer race spacer',
'Outer race spacer',(#5686));
#5666=PRODUCT_RELATED_PRODUCT_CATEGORY('Seal cap','Seal cap',(#5687));
#5667=PRODUCT_RELATED_PRODUCT_CATEGORY('Dust seal envelope',
'Dust seal envelope',(#5688));
#5668=PRODUCT_RELATED_PRODUCT_CATEGORY('Rear cap','Rear cap',(#5689));
#5669=PRODUCT_RELATED_PRODUCT_CATEGORY('Cap Screw - M4x16',
'Cap Screw - M4x16',(#5690));
#5670=PRODUCT_RELATED_PRODUCT_CATEGORY(
'Shaft spacer and retaining ring','Shaft spacer and retaining ring',(#5691));
#5671=PRODUCT_RELATED_PRODUCT_CATEGORY('Retained shaft',
'Retained shaft',(#5692));
#5672=PRODUCT_RELATED_PRODUCT_CATEGORY('Inner race spacer',
'Inner race spacer',(#5693));
#5673=PRODUCT_RELATED_PRODUCT_CATEGORY('Installed retaining ring',
'Installed retaining ring',(#5694));
#5674=APPLICATION_PROTOCOL_DEFINITION('international standard',
'automotive_design',2009,#5675);
#5675=APPLICATION_CONTEXT(
'Core Data for Automotive Mechanical Design Process');
#5676=PRODUCT_CONTEXT('part definition',#5675,'mechanical');
#5677=PRODUCT('PAT-030','PAT-030',
'PAT-030',(#5676));
#5678=PRODUCT('Flanged housing bearings and seal caps',
'Flanged housing bearings and seal caps',
'Flanged housing bearings and seal caps',(#5676));
#5679=PRODUCT('Flanged housing','Flanged housing','Flanged housing',(#5676));
#5680=PRODUCT('Sealed Ball Bearing - 20 x 47 x 14 mm',
'Sealed Ball Bearing - 20 x 47 x 14 mm',
'Sealed Ball Bearing - 20 x 47 x 14 mm',(#5676));
#5681=PRODUCT('Inner ring','Inner ring','Inner ring',(#5676));
#5682=PRODUCT('Outer ring','Outer ring','Outer ring',(#5676));
#5683=PRODUCT('Balls','Balls','Balls',(#5676));
#5684=PRODUCT('Cage','Cage','Cage',(#5676));
#5685=PRODUCT('Seals 2RS','Seals 2RS','Seals 2RS',(#5676));
#5686=PRODUCT('Outer race spacer','Outer race spacer',
'Outer race spacer',(#5676));
#5687=PRODUCT('Seal cap','Seal cap','Seal cap',(#5676));
#5688=PRODUCT('Dust seal envelope','Dust seal envelope',
'Dust seal envelope',(#5676));
#5689=PRODUCT('Rear cap','Rear cap','Rear cap',(#5676));
#5690=PRODUCT('Cap Screw - M4x16','Cap Screw - M4x16',
'Cap Screw - M4x16',(#5676));
#5691=PRODUCT('Shaft spacer and retaining ring',
'Shaft spacer and retaining ring','Shaft spacer and retaining ring',(#5676));
#5692=PRODUCT('Retained shaft','Retained shaft','Retained shaft',(#5676));
#5693=PRODUCT('Inner race spacer','Inner race spacer',
'Inner race spacer',(#5676));
#5694=PRODUCT('Installed retaining ring','Installed retaining ring',
'Installed retaining ring',(#5676));
#5695=PRESENTATION_STYLE_ASSIGNMENT((#5701));
#5696=PRESENTATION_STYLE_ASSIGNMENT((#5702));
#5697=PRESENTATION_STYLE_ASSIGNMENT((#5703));
#5698=PRESENTATION_STYLE_ASSIGNMENT((#5704));
#5699=PRESENTATION_STYLE_ASSIGNMENT((#5705));
#5700=PRESENTATION_STYLE_ASSIGNMENT((#5706));
#5701=SURFACE_STYLE_USAGE(.BOTH.,#5707);
#5702=SURFACE_STYLE_USAGE(.BOTH.,#5708);
#5703=SURFACE_STYLE_USAGE(.BOTH.,#5709);
#5704=SURFACE_STYLE_USAGE(.BOTH.,#5710);
#5705=SURFACE_STYLE_USAGE(.BOTH.,#5711);
#5706=SURFACE_STYLE_USAGE(.BOTH.,#5712);
#5707=SURFACE_SIDE_STYLE('',(#5713));
#5708=SURFACE_SIDE_STYLE('',(#5714));
#5709=SURFACE_SIDE_STYLE('',(#5715));
#5710=SURFACE_SIDE_STYLE('',(#5716));
#5711=SURFACE_SIDE_STYLE('',(#5717));
#5712=SURFACE_SIDE_STYLE('',(#5718));
#5713=SURFACE_STYLE_FILL_AREA(#5719);
#5714=SURFACE_STYLE_FILL_AREA(#5720);
#5715=SURFACE_STYLE_FILL_AREA(#5721);
#5716=SURFACE_STYLE_FILL_AREA(#5722);
#5717=SURFACE_STYLE_FILL_AREA(#5723);
#5718=SURFACE_STYLE_FILL_AREA(#5724);
#5719=FILL_AREA_STYLE('Steel - Satin',(#5725));
#5720=FILL_AREA_STYLE('CAD Library Painted - Light blue',(#5726));
#5721=FILL_AREA_STYLE('CAD Library Painted - Steel gray',(#5727));
#5722=FILL_AREA_STYLE('CAD Library Painted - Engineering blue',(#5728));
#5723=FILL_AREA_STYLE('CAD Library Painted - Off white',(#5729));
#5724=FILL_AREA_STYLE('CAD Library Painted - Graphite',(#5730));
#5725=FILL_AREA_STYLE_COLOUR('Steel - Satin',#5731);
#5726=FILL_AREA_STYLE_COLOUR('CAD Library Painted - Light blue',#5732);
#5727=FILL_AREA_STYLE_COLOUR('CAD Library Painted - Steel gray',#5733);
#5728=FILL_AREA_STYLE_COLOUR('CAD Library Painted - Engineering blue',#5734);
#5729=FILL_AREA_STYLE_COLOUR('CAD Library Painted - Off white',#5735);
#5730=FILL_AREA_STYLE_COLOUR('CAD Library Painted - Graphite',#5736);
#5731=COLOUR_RGB('Steel - Satin',0.627450980392157,0.627450980392157,0.627450980392157);
#5732=COLOUR_RGB('CAD Library Painted - Light blue',0.286274509803922,0.552941176470588,
0.780392156862745);
#5733=COLOUR_RGB('CAD Library Painted - Steel gray',0.592156862745098,0.631372549019608,
0.67843137254902);
#5734=COLOUR_RGB('CAD Library Painted - Engineering blue',0.12156862745098,
0.356862745098039,0.6);
#5735=COLOUR_RGB('CAD Library Painted - Off white',0.909803921568627,0.901960784313726,
0.858823529411765);
#5736=COLOUR_RGB('CAD Library Painted - Graphite',0.0980392156862745,0.109803921568627,
0.125490196078431);
#5737=COLOUR_RGB('Dark Blue',0.08,0.2,0.34);
#5738=FILL_AREA_STYLE_COLOUR('',#5737);
#5739=FILL_AREA_STYLE('',(#5738));
#5740=SURFACE_STYLE_FILL_AREA(#5739);
#5741=SURFACE_SIDE_STYLE('',(#5740));
#5742=SURFACE_STYLE_USAGE(.BOTH.,#5741);
#5743=PRESENTATION_STYLE_ASSIGNMENT((#5742));
#5744=COLOUR_RGB('Light Blue',0.38,0.62,0.78);
#5745=FILL_AREA_STYLE_COLOUR('',#5744);
#5746=FILL_AREA_STYLE('',(#5745));
#5747=SURFACE_STYLE_FILL_AREA(#5746);
#5748=SURFACE_SIDE_STYLE('',(#5747));
#5749=SURFACE_STYLE_USAGE(.BOTH.,#5748);
#5750=PRESENTATION_STYLE_ASSIGNMENT((#5749));
#5751=COLOUR_RGB('Sky Blue',0.24,0.69,0.87);
#5752=FILL_AREA_STYLE_COLOUR('',#5751);
#5753=FILL_AREA_STYLE('',(#5752));
#5754=SURFACE_STYLE_FILL_AREA(#5753);
#5755=SURFACE_SIDE_STYLE('',(#5754));
#5756=SURFACE_STYLE_USAGE(.BOTH.,#5755);
#5757=PRESENTATION_STYLE_ASSIGNMENT((#5756));
#5758=COLOUR_RGB('Grey',0.48,0.52,0.57);
#5759=FILL_AREA_STYLE_COLOUR('',#5758);
#5760=FILL_AREA_STYLE('',(#5759));
#5761=SURFACE_STYLE_FILL_AREA(#5760);
#5762=SURFACE_SIDE_STYLE('',(#5761));
#5763=SURFACE_STYLE_USAGE(.BOTH.,#5762);
#5764=PRESENTATION_STYLE_ASSIGNMENT((#5763));
#5765=COLOUR_RGB('Black',0.12,0.14,0.17);
#5766=FILL_AREA_STYLE_COLOUR('',#5765);
#5767=FILL_AREA_STYLE('',(#5766));
#5768=SURFACE_STYLE_FILL_AREA(#5767);
#5769=SURFACE_SIDE_STYLE('',(#5768));
#5770=SURFACE_STYLE_USAGE(.BOTH.,#5769);
#5771=PRESENTATION_STYLE_ASSIGNMENT((#5770));
#5772=COLOUR_RGB('Off White',0.89,0.88,0.83);
#5773=FILL_AREA_STYLE_COLOUR('',#5772);
#5774=FILL_AREA_STYLE('',(#5773));
#5775=SURFACE_STYLE_FILL_AREA(#5774);
#5776=SURFACE_SIDE_STYLE('',(#5775));
#5777=SURFACE_STYLE_USAGE(.BOTH.,#5776);
#5778=PRESENTATION_STYLE_ASSIGNMENT((#5777));
ENDSEC;
END-ISO-10303-21;
